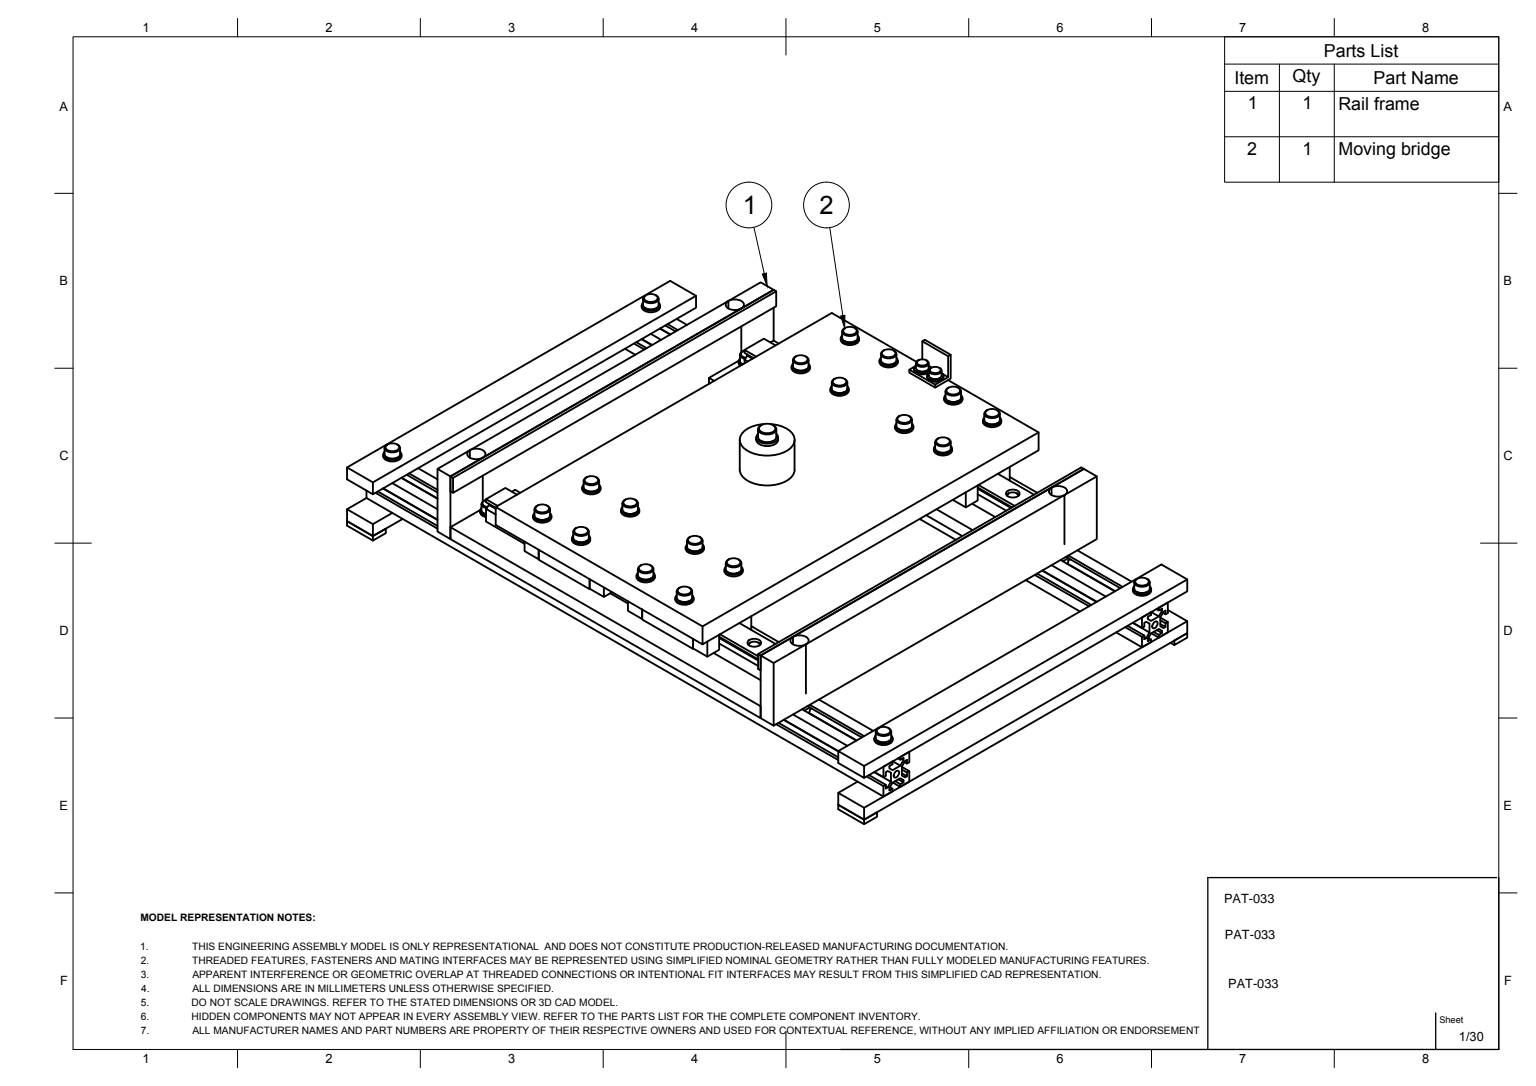
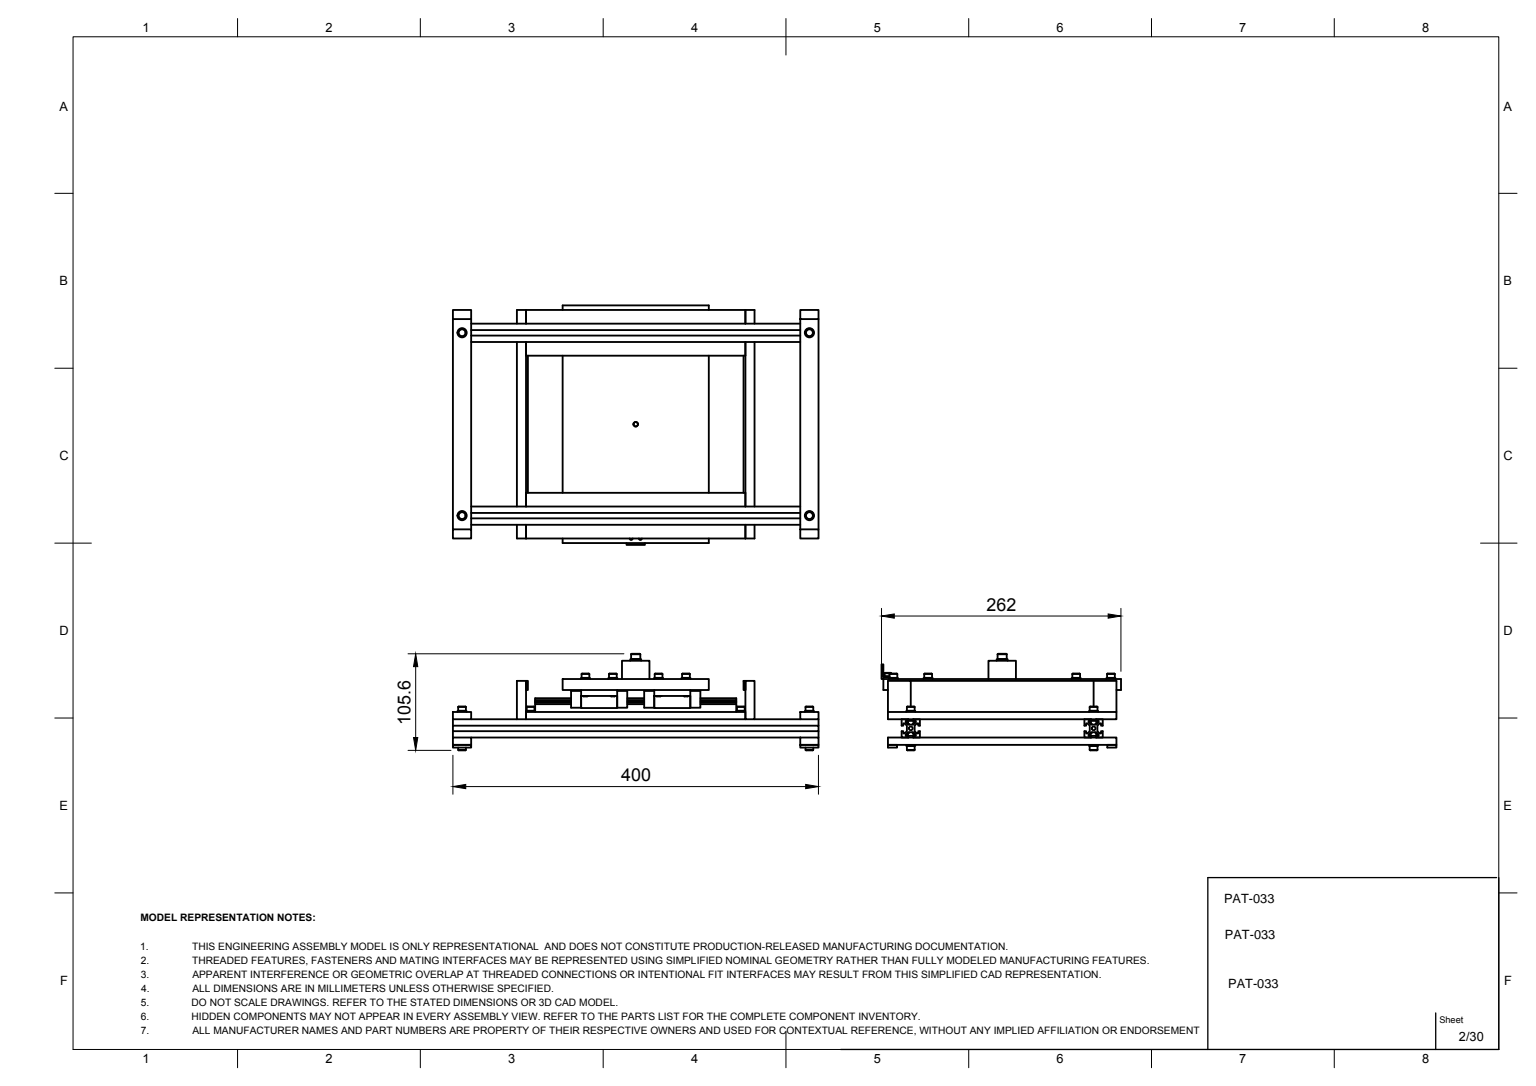
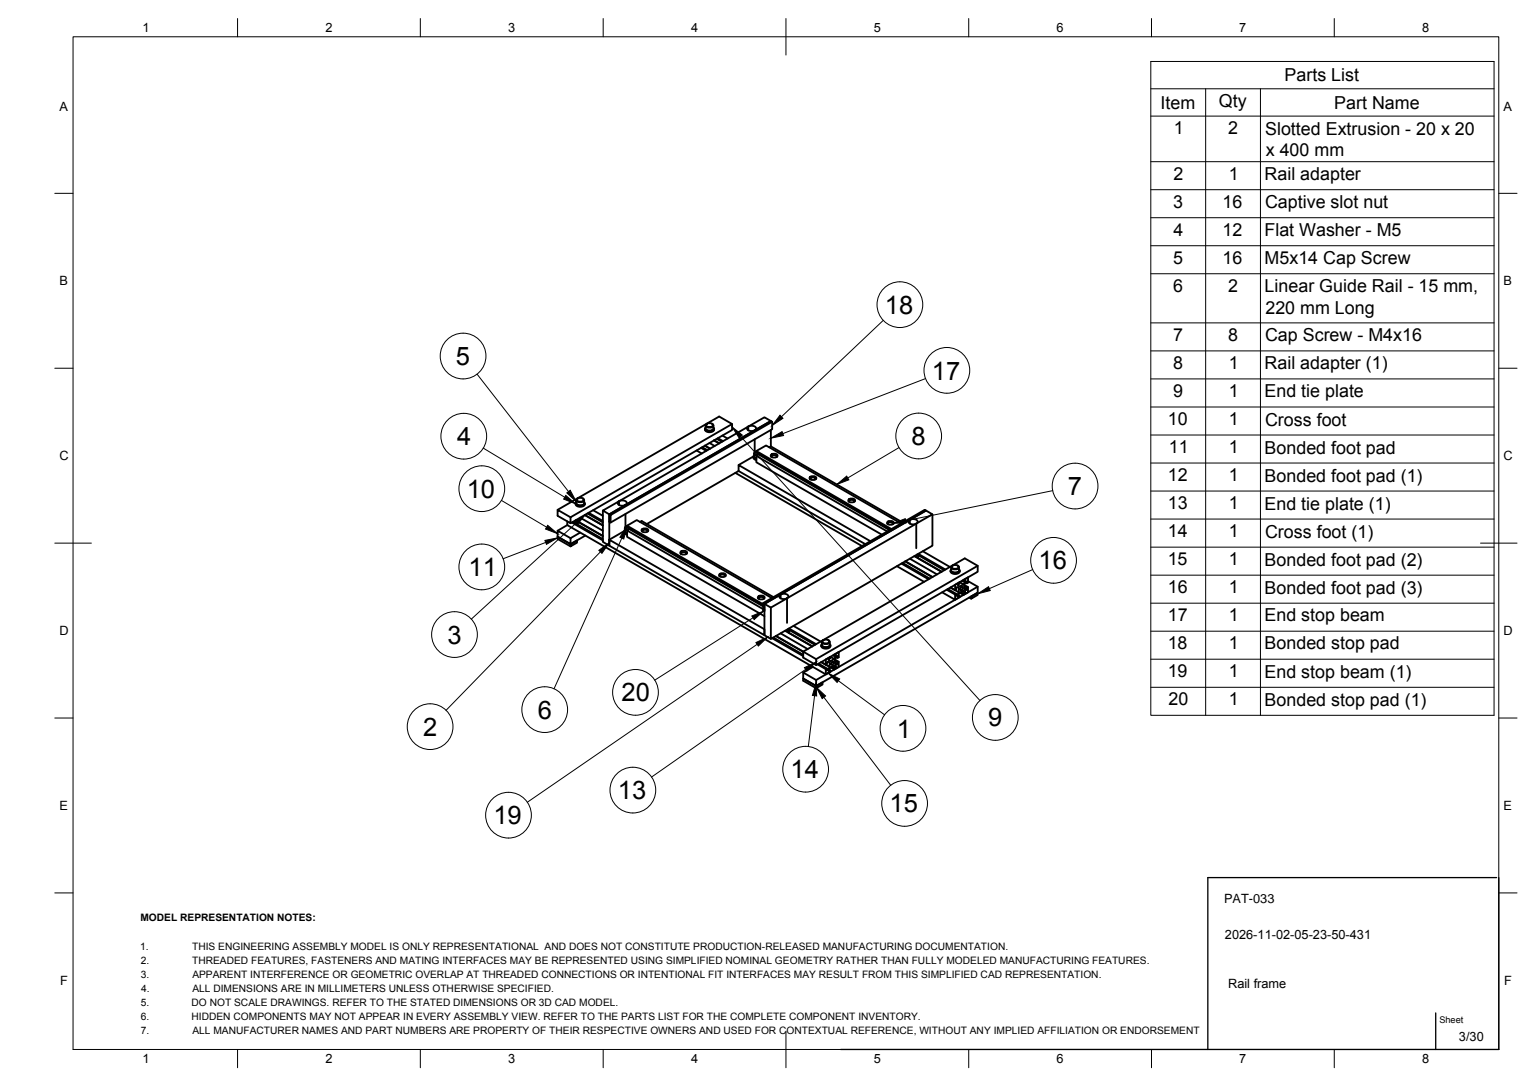
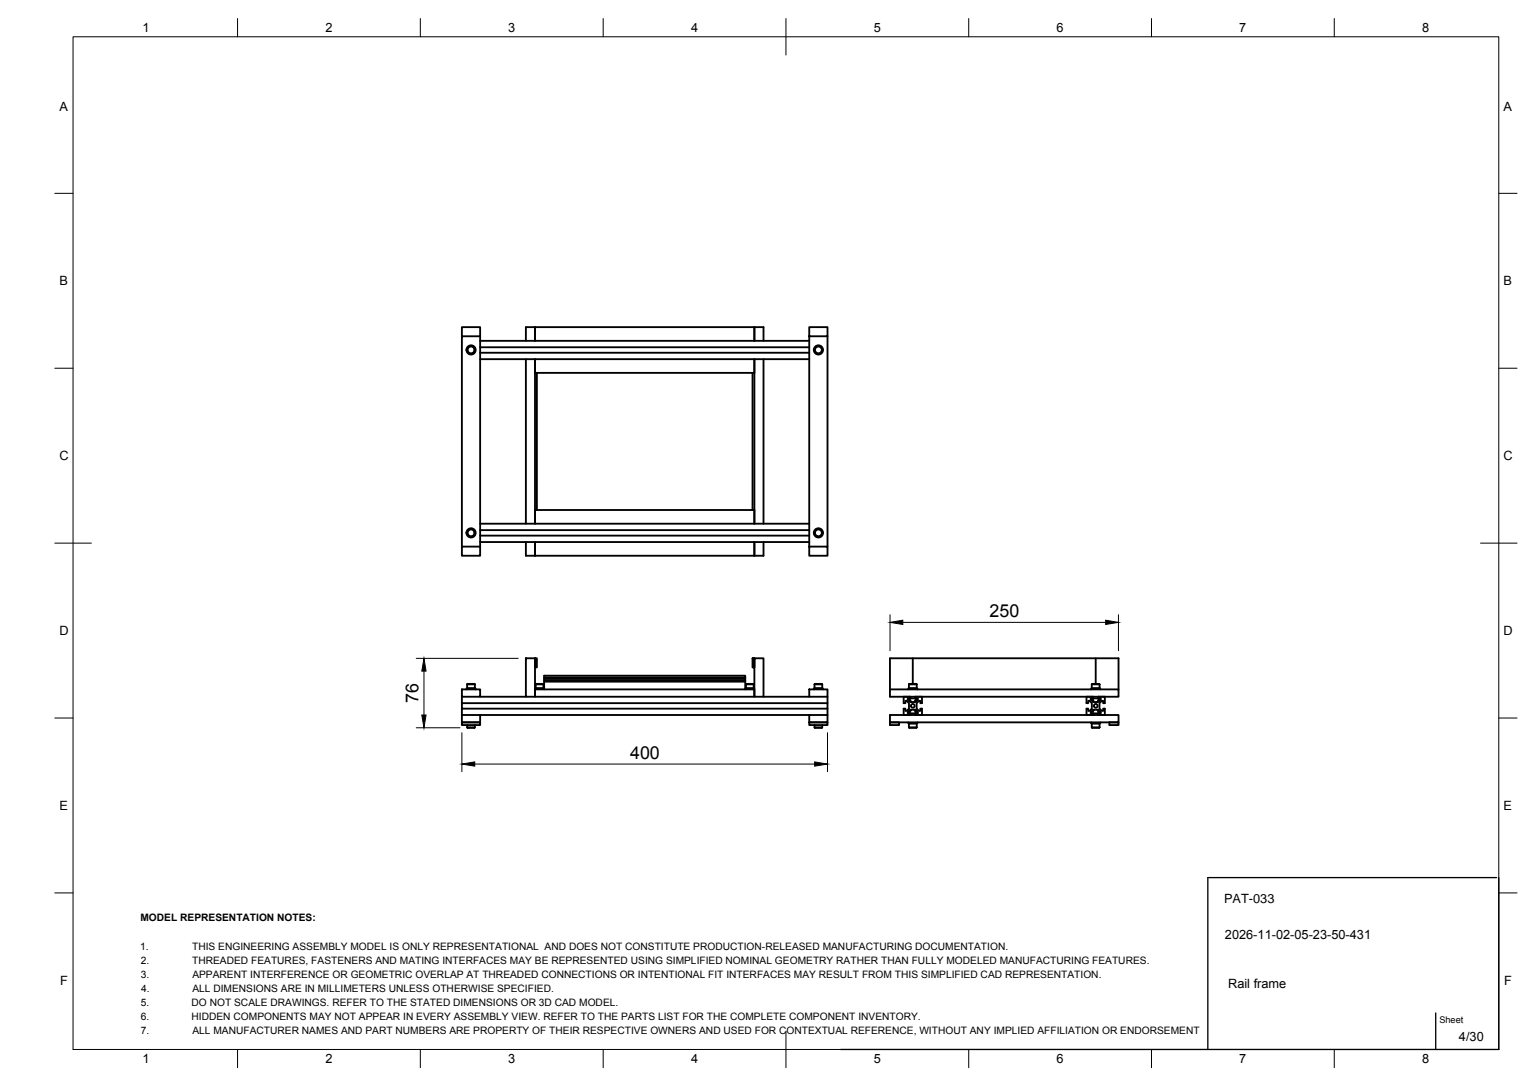
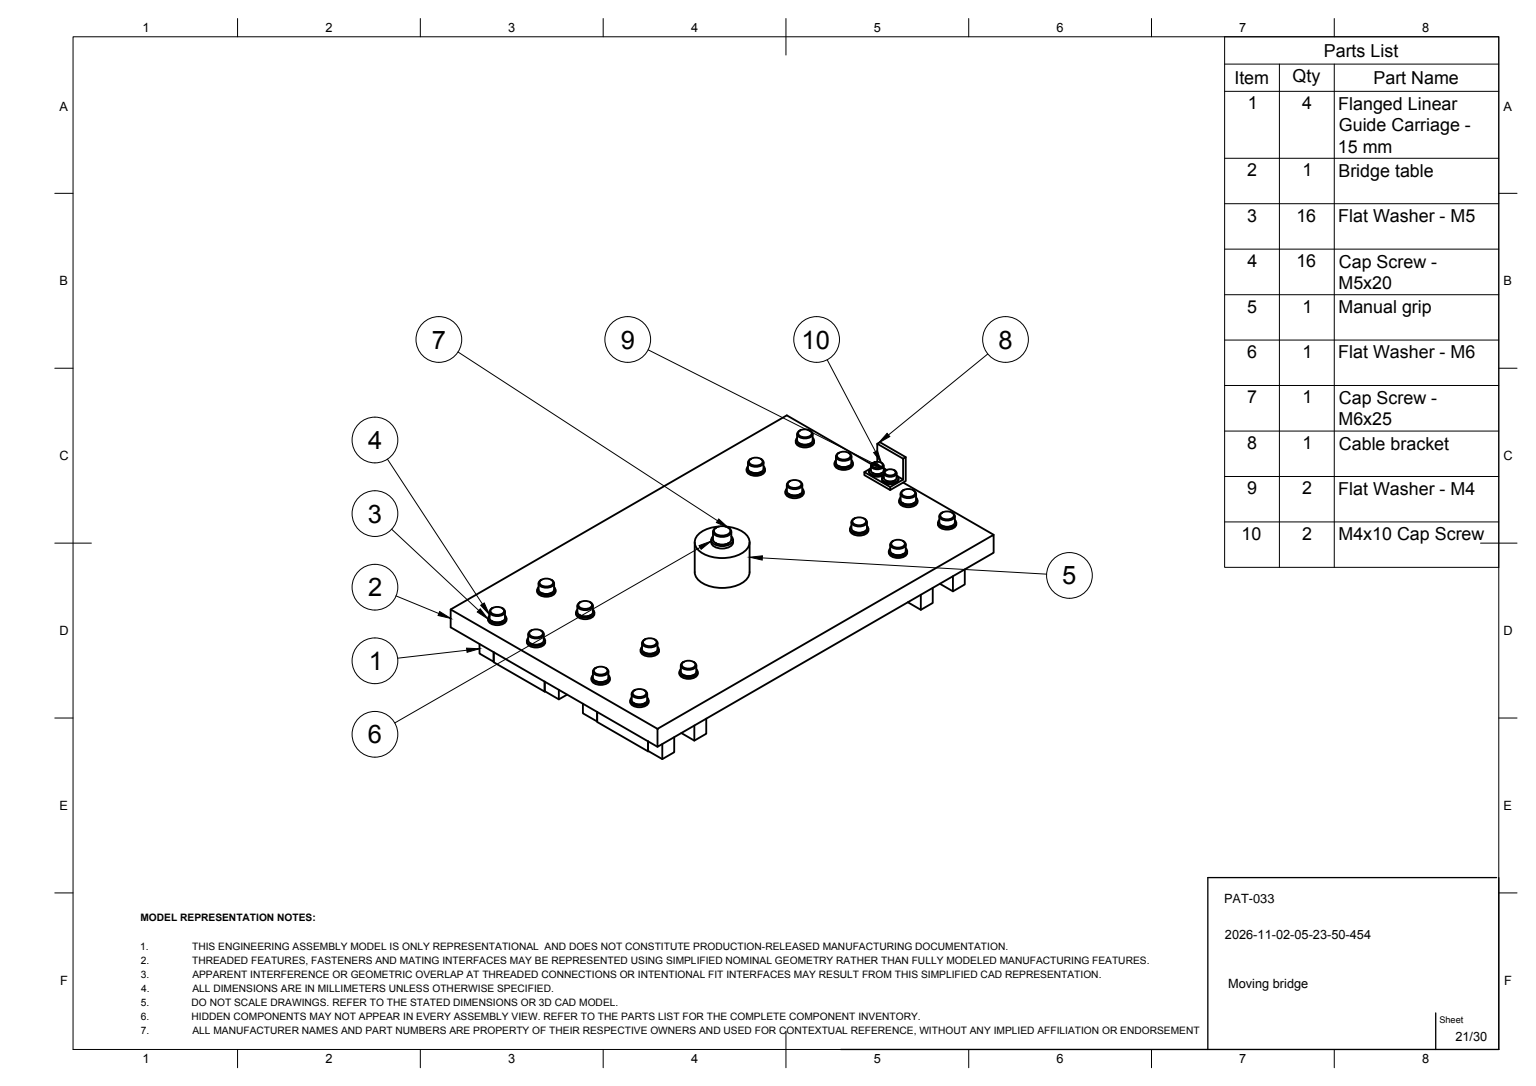
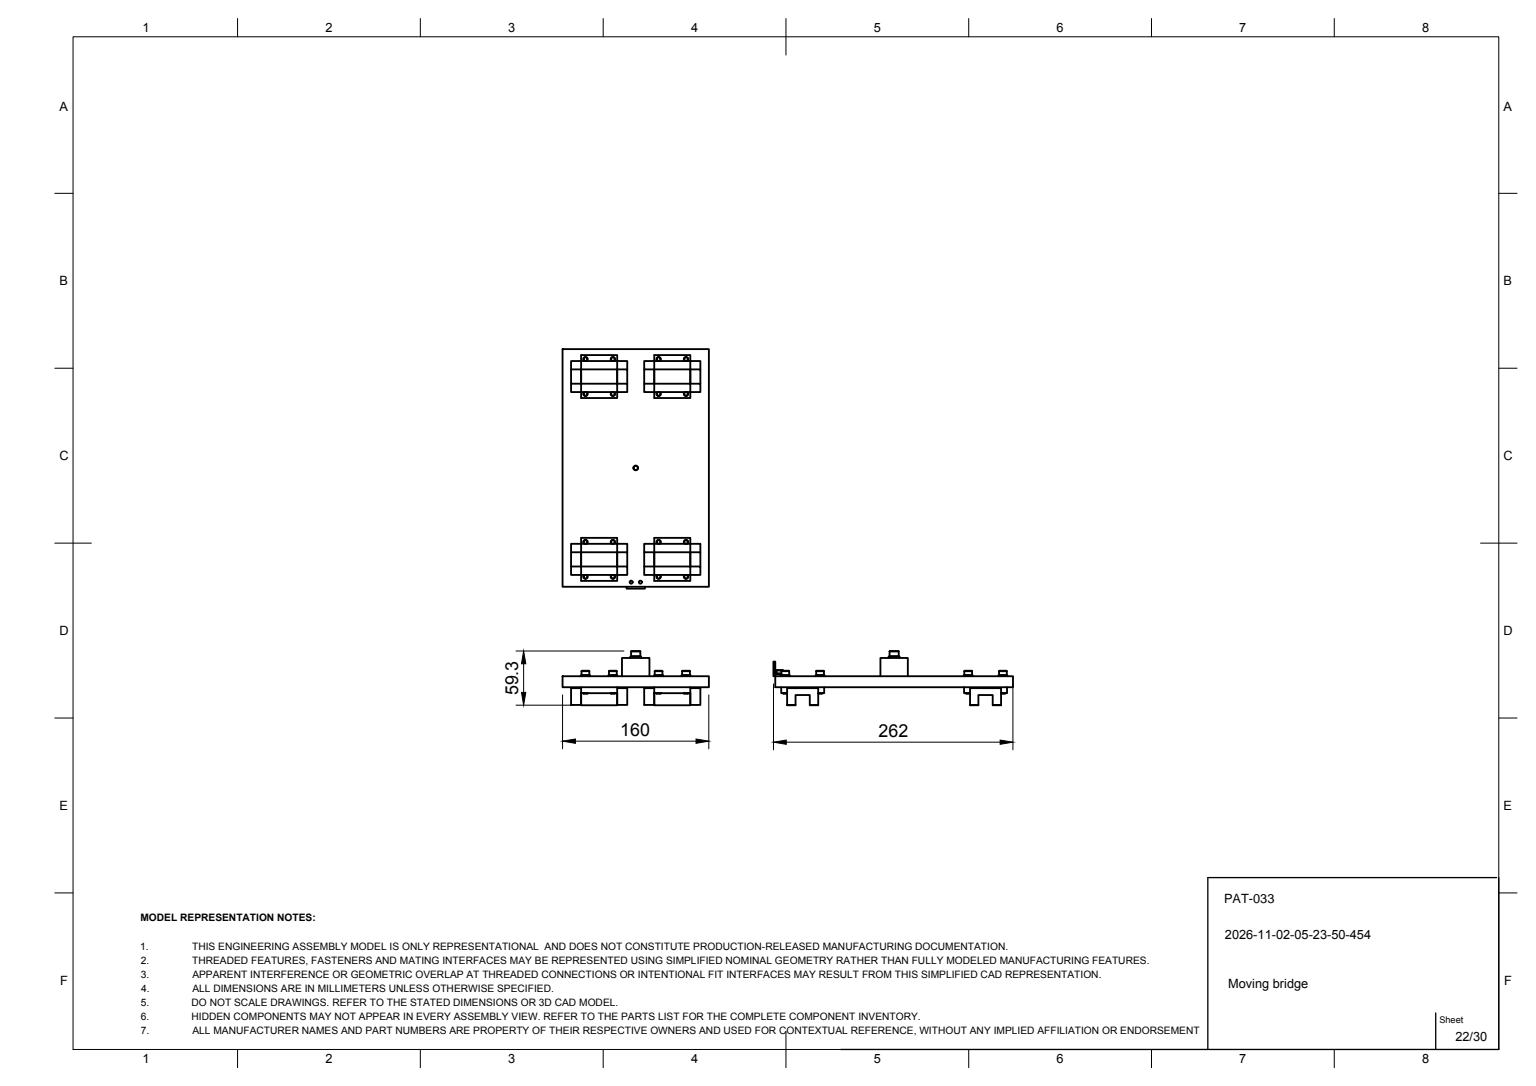
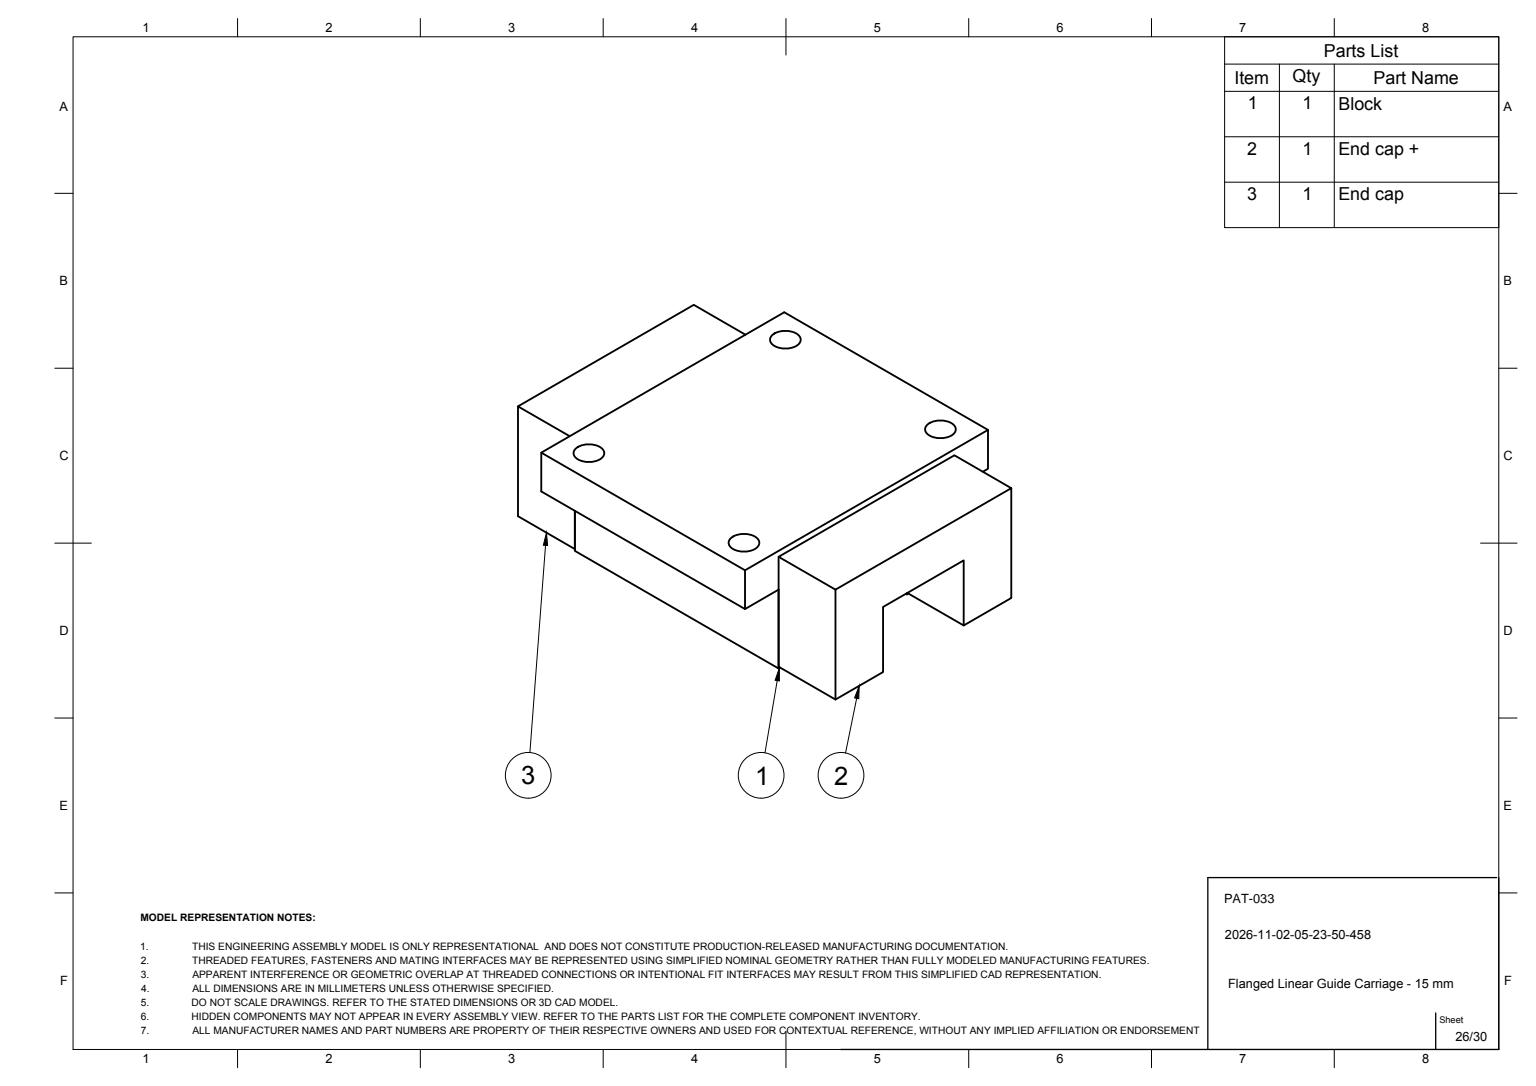
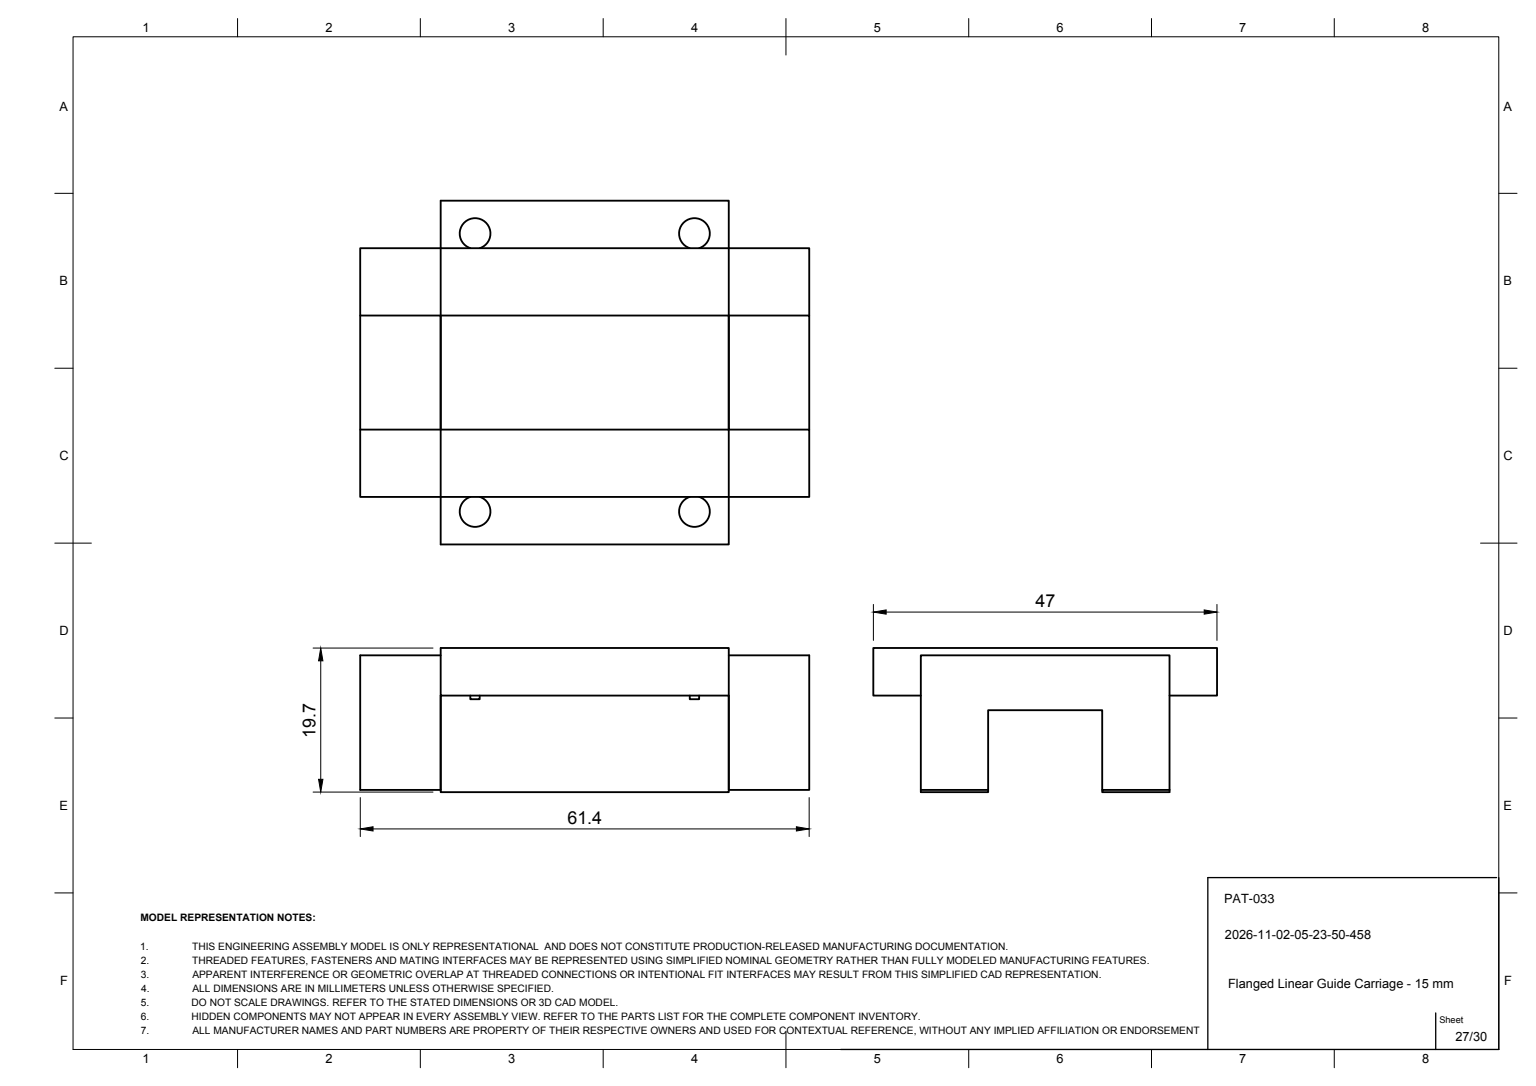
ISO-10303-21;
HEADER;
/* Generated by software containing ST-Developer
 * from STEP Tools, Inc. (www.steptools.com) 
 */

FILE_DESCRIPTION(
/* description */ ('Dual-rail gantry carriage'),
/* implementation_level */ '2;1');

FILE_NAME(
/* name */ 'PAT-033',
/* time_stamp */ '2026-10-27T10:49:15-07:00',
/* author */ (''),
/* organization */ (''),
/* preprocessor_version */ 'ST-DEVELOPER v20.2',
/* originating_system */ 'Autodesk Translation Framework v15.17.0.0',
/* authorisation */ '');

FILE_SCHEMA (('AUTOMOTIVE_DESIGN { 1 0 10303 214 3 1 1 }'));
ENDSEC;

DATA;
#10=MECHANICAL_DESIGN_GEOMETRIC_PRESENTATION_REPRESENTATION('',(#585,#586,
#587,#588,#589,#590,#591,#592,#593,#594,#595,#596,#597,#598,#599,#600,#601,
#602,#603,#604,#605,#606,#607,#608,#609,#610,#611,#612,#613,#614,#615),
#12804);
#11=ITEM_DEFINED_TRANSFORMATION($,$,#8199,#8260);
#12=ITEM_DEFINED_TRANSFORMATION($,$,#8238,#8261);
#13=ITEM_DEFINED_TRANSFORMATION($,$,#8249,#8262);
#14=ITEM_DEFINED_TRANSFORMATION($,$,#7743,#8274);
#15=ITEM_DEFINED_TRANSFORMATION($,$,#7768,#8275);
#16=ITEM_DEFINED_TRANSFORMATION($,$,#7793,#8276);
#17=ITEM_DEFINED_TRANSFORMATION($,$,#7806,#8277);
#18=ITEM_DEFINED_TRANSFORMATION($,$,#7819,#8278);
#19=ITEM_DEFINED_TRANSFORMATION($,$,#7826,#8279);
#20=ITEM_DEFINED_TRANSFORMATION($,$,#7833,#8280);
#21=ITEM_DEFINED_TRANSFORMATION($,$,#7846,#8281);
#22=ITEM_DEFINED_TRANSFORMATION($,$,#7859,#8282);
#23=ITEM_DEFINED_TRANSFORMATION($,$,#7866,#8283);
#24=ITEM_DEFINED_TRANSFORMATION($,$,#7873,#8284);
#25=ITEM_DEFINED_TRANSFORMATION($,$,#7902,#8285);
#26=ITEM_DEFINED_TRANSFORMATION($,$,#7909,#8286);
#27=ITEM_DEFINED_TRANSFORMATION($,$,#7938,#8287);
#28=ITEM_DEFINED_TRANSFORMATION($,$,#7945,#8288);
#29=ITEM_DEFINED_TRANSFORMATION($,$,#8064,#8289);
#30=ITEM_DEFINED_TRANSFORMATION($,$,#8263,#8290);
#31=ITEM_DEFINED_TRANSFORMATION($,$,#8085,#8291);
#32=ITEM_DEFINED_TRANSFORMATION($,$,#8064,#8292);
#33=ITEM_DEFINED_TRANSFORMATION($,$,#8263,#8293);
#34=ITEM_DEFINED_TRANSFORMATION($,$,#8085,#8294);
#35=ITEM_DEFINED_TRANSFORMATION($,$,#7995,#8295);
#36=ITEM_DEFINED_TRANSFORMATION($,$,#8038,#8296);
#37=ITEM_DEFINED_TRANSFORMATION($,$,#8038,#8297);
#38=ITEM_DEFINED_TRANSFORMATION($,$,#8038,#8298);
#39=ITEM_DEFINED_TRANSFORMATION($,$,#8038,#8299);
#40=ITEM_DEFINED_TRANSFORMATION($,$,#7945,#8300);
#41=ITEM_DEFINED_TRANSFORMATION($,$,#8064,#8301);
#42=ITEM_DEFINED_TRANSFORMATION($,$,#8263,#8302);
#43=ITEM_DEFINED_TRANSFORMATION($,$,#8085,#8303);
#44=ITEM_DEFINED_TRANSFORMATION($,$,#8064,#8304);
#45=ITEM_DEFINED_TRANSFORMATION($,$,#8263,#8305);
#46=ITEM_DEFINED_TRANSFORMATION($,$,#8085,#8306);
#47=ITEM_DEFINED_TRANSFORMATION($,$,#7995,#8307);
#48=ITEM_DEFINED_TRANSFORMATION($,$,#8038,#8308);
#49=ITEM_DEFINED_TRANSFORMATION($,$,#8038,#8309);
#50=ITEM_DEFINED_TRANSFORMATION($,$,#8038,#8310);
#51=ITEM_DEFINED_TRANSFORMATION($,$,#8038,#8311);
#52=ITEM_DEFINED_TRANSFORMATION($,$,#8064,#8312);
#53=ITEM_DEFINED_TRANSFORMATION($,$,#8263,#8313);
#54=ITEM_DEFINED_TRANSFORMATION($,$,#8085,#8314);
#55=ITEM_DEFINED_TRANSFORMATION($,$,#8064,#8315);
#56=ITEM_DEFINED_TRANSFORMATION($,$,#8263,#8316);
#57=ITEM_DEFINED_TRANSFORMATION($,$,#8085,#8317);
#58=ITEM_DEFINED_TRANSFORMATION($,$,#8064,#8318);
#59=ITEM_DEFINED_TRANSFORMATION($,$,#8263,#8319);
#60=ITEM_DEFINED_TRANSFORMATION($,$,#8085,#8320);
#61=ITEM_DEFINED_TRANSFORMATION($,$,#8064,#8321);
#62=ITEM_DEFINED_TRANSFORMATION($,$,#8263,#8322);
#63=ITEM_DEFINED_TRANSFORMATION($,$,#8085,#8323);
#64=ITEM_DEFINED_TRANSFORMATION($,$,#8064,#8324);
#65=ITEM_DEFINED_TRANSFORMATION($,$,#8263,#8325);
#66=ITEM_DEFINED_TRANSFORMATION($,$,#8085,#8326);
#67=ITEM_DEFINED_TRANSFORMATION($,$,#8064,#8327);
#68=ITEM_DEFINED_TRANSFORMATION($,$,#8263,#8328);
#69=ITEM_DEFINED_TRANSFORMATION($,$,#8085,#8329);
#70=ITEM_DEFINED_TRANSFORMATION($,$,#8064,#8330);
#71=ITEM_DEFINED_TRANSFORMATION($,$,#8263,#8331);
#72=ITEM_DEFINED_TRANSFORMATION($,$,#8085,#8332);
#73=ITEM_DEFINED_TRANSFORMATION($,$,#8064,#8333);
#74=ITEM_DEFINED_TRANSFORMATION($,$,#8263,#8334);
#75=ITEM_DEFINED_TRANSFORMATION($,$,#8085,#8335);
#76=ITEM_DEFINED_TRANSFORMATION($,$,#8064,#8336);
#77=ITEM_DEFINED_TRANSFORMATION($,$,#8085,#8337);
#78=ITEM_DEFINED_TRANSFORMATION($,$,#8064,#8338);
#79=ITEM_DEFINED_TRANSFORMATION($,$,#8085,#8339);
#80=ITEM_DEFINED_TRANSFORMATION($,$,#8064,#8340);
#81=ITEM_DEFINED_TRANSFORMATION($,$,#8085,#8341);
#82=ITEM_DEFINED_TRANSFORMATION($,$,#8064,#8342);
#83=ITEM_DEFINED_TRANSFORMATION($,$,#8085,#8343);
#84=ITEM_DEFINED_TRANSFORMATION($,$,#8110,#8440);
#85=ITEM_DEFINED_TRANSFORMATION($,$,#8174,#8441);
#86=ITEM_DEFINED_TRANSFORMATION($,$,#8183,#8442);
#87=ITEM_DEFINED_TRANSFORMATION($,$,#8198,#8443);
#88=ITEM_DEFINED_TRANSFORMATION($,$,#8198,#8444);
#89=ITEM_DEFINED_TRANSFORMATION($,$,#8198,#8445);
#90=ITEM_DEFINED_TRANSFORMATION($,$,#8198,#8446);
#91=ITEM_DEFINED_TRANSFORMATION($,$,#8263,#8447);
#92=ITEM_DEFINED_TRANSFORMATION($,$,#8344,#8448);
#93=ITEM_DEFINED_TRANSFORMATION($,$,#8263,#8449);
#94=ITEM_DEFINED_TRANSFORMATION($,$,#8344,#8450);
#95=ITEM_DEFINED_TRANSFORMATION($,$,#8263,#8451);
#96=ITEM_DEFINED_TRANSFORMATION($,$,#8344,#8452);
#97=ITEM_DEFINED_TRANSFORMATION($,$,#8263,#8453);
#98=ITEM_DEFINED_TRANSFORMATION($,$,#8344,#8454);
#99=ITEM_DEFINED_TRANSFORMATION($,$,#8263,#8455);
#100=ITEM_DEFINED_TRANSFORMATION($,$,#8344,#8456);
#101=ITEM_DEFINED_TRANSFORMATION($,$,#8263,#8457);
#102=ITEM_DEFINED_TRANSFORMATION($,$,#8344,#8458);
#103=ITEM_DEFINED_TRANSFORMATION($,$,#8263,#8459);
#104=ITEM_DEFINED_TRANSFORMATION($,$,#8344,#8460);
#105=ITEM_DEFINED_TRANSFORMATION($,$,#8263,#8461);
#106=ITEM_DEFINED_TRANSFORMATION($,$,#8344,#8462);
#107=ITEM_DEFINED_TRANSFORMATION($,$,#8263,#8463);
#108=ITEM_DEFINED_TRANSFORMATION($,$,#8344,#8464);
#109=ITEM_DEFINED_TRANSFORMATION($,$,#8263,#8465);
#110=ITEM_DEFINED_TRANSFORMATION($,$,#8344,#8466);
#111=ITEM_DEFINED_TRANSFORMATION($,$,#8263,#8467);
#112=ITEM_DEFINED_TRANSFORMATION($,$,#8344,#8468);
#113=ITEM_DEFINED_TRANSFORMATION($,$,#8263,#8469);
#114=ITEM_DEFINED_TRANSFORMATION($,$,#8344,#8470);
#115=ITEM_DEFINED_TRANSFORMATION($,$,#8263,#8471);
#116=ITEM_DEFINED_TRANSFORMATION($,$,#8344,#8472);
#117=ITEM_DEFINED_TRANSFORMATION($,$,#8263,#8473);
#118=ITEM_DEFINED_TRANSFORMATION($,$,#8344,#8474);
#119=ITEM_DEFINED_TRANSFORMATION($,$,#8263,#8475);
#120=ITEM_DEFINED_TRANSFORMATION($,$,#8344,#8476);
#121=ITEM_DEFINED_TRANSFORMATION($,$,#8263,#8477);
#122=ITEM_DEFINED_TRANSFORMATION($,$,#8344,#8478);
#123=ITEM_DEFINED_TRANSFORMATION($,$,#8370,#8479);
#124=ITEM_DEFINED_TRANSFORMATION($,$,#8379,#8480);
#125=ITEM_DEFINED_TRANSFORMATION($,$,#8405,#8481);
#126=ITEM_DEFINED_TRANSFORMATION($,$,#8416,#8482);
#127=ITEM_DEFINED_TRANSFORMATION($,$,#8405,#8483);
#128=ITEM_DEFINED_TRANSFORMATION($,$,#8416,#8484);
#129=ITEM_DEFINED_TRANSFORMATION($,$,#7742,#8485);
#130=ITEM_DEFINED_TRANSFORMATION($,$,#8109,#8486);
#131=(
REPRESENTATION_RELATIONSHIP($,$,#13025,#13024)
REPRESENTATION_RELATIONSHIP_WITH_TRANSFORMATION(#11)
SHAPE_REPRESENTATION_RELATIONSHIP()
);
#132=(
REPRESENTATION_RELATIONSHIP($,$,#13026,#13024)
REPRESENTATION_RELATIONSHIP_WITH_TRANSFORMATION(#12)
SHAPE_REPRESENTATION_RELATIONSHIP()
);
#133=(
REPRESENTATION_RELATIONSHIP($,$,#13027,#13024)
REPRESENTATION_RELATIONSHIP_WITH_TRANSFORMATION(#13)
SHAPE_REPRESENTATION_RELATIONSHIP()
);
#134=(
REPRESENTATION_RELATIONSHIP($,$,#13001,#13000)
REPRESENTATION_RELATIONSHIP_WITH_TRANSFORMATION(#14)
SHAPE_REPRESENTATION_RELATIONSHIP()
);
#135=(
REPRESENTATION_RELATIONSHIP($,$,#13002,#13000)
REPRESENTATION_RELATIONSHIP_WITH_TRANSFORMATION(#15)
SHAPE_REPRESENTATION_RELATIONSHIP()
);
#136=(
REPRESENTATION_RELATIONSHIP($,$,#13003,#13000)
REPRESENTATION_RELATIONSHIP_WITH_TRANSFORMATION(#16)
SHAPE_REPRESENTATION_RELATIONSHIP()
);
#137=(
REPRESENTATION_RELATIONSHIP($,$,#13004,#13000)
REPRESENTATION_RELATIONSHIP_WITH_TRANSFORMATION(#17)
SHAPE_REPRESENTATION_RELATIONSHIP()
);
#138=(
REPRESENTATION_RELATIONSHIP($,$,#13005,#13000)
REPRESENTATION_RELATIONSHIP_WITH_TRANSFORMATION(#18)
SHAPE_REPRESENTATION_RELATIONSHIP()
);
#139=(
REPRESENTATION_RELATIONSHIP($,$,#13006,#13000)
REPRESENTATION_RELATIONSHIP_WITH_TRANSFORMATION(#19)
SHAPE_REPRESENTATION_RELATIONSHIP()
);
#140=(
REPRESENTATION_RELATIONSHIP($,$,#13007,#13000)
REPRESENTATION_RELATIONSHIP_WITH_TRANSFORMATION(#20)
SHAPE_REPRESENTATION_RELATIONSHIP()
);
#141=(
REPRESENTATION_RELATIONSHIP($,$,#13008,#13000)
REPRESENTATION_RELATIONSHIP_WITH_TRANSFORMATION(#21)
SHAPE_REPRESENTATION_RELATIONSHIP()
);
#142=(
REPRESENTATION_RELATIONSHIP($,$,#13009,#13000)
REPRESENTATION_RELATIONSHIP_WITH_TRANSFORMATION(#22)
SHAPE_REPRESENTATION_RELATIONSHIP()
);
#143=(
REPRESENTATION_RELATIONSHIP($,$,#13010,#13000)
REPRESENTATION_RELATIONSHIP_WITH_TRANSFORMATION(#23)
SHAPE_REPRESENTATION_RELATIONSHIP()
);
#144=(
REPRESENTATION_RELATIONSHIP($,$,#13011,#13000)
REPRESENTATION_RELATIONSHIP_WITH_TRANSFORMATION(#24)
SHAPE_REPRESENTATION_RELATIONSHIP()
);
#145=(
REPRESENTATION_RELATIONSHIP($,$,#13012,#13000)
REPRESENTATION_RELATIONSHIP_WITH_TRANSFORMATION(#25)
SHAPE_REPRESENTATION_RELATIONSHIP()
);
#146=(
REPRESENTATION_RELATIONSHIP($,$,#13013,#13000)
REPRESENTATION_RELATIONSHIP_WITH_TRANSFORMATION(#26)
SHAPE_REPRESENTATION_RELATIONSHIP()
);
#147=(
REPRESENTATION_RELATIONSHIP($,$,#13014,#13000)
REPRESENTATION_RELATIONSHIP_WITH_TRANSFORMATION(#27)
SHAPE_REPRESENTATION_RELATIONSHIP()
);
#148=(
REPRESENTATION_RELATIONSHIP($,$,#13015,#13000)
REPRESENTATION_RELATIONSHIP_WITH_TRANSFORMATION(#28)
SHAPE_REPRESENTATION_RELATIONSHIP()
);
#149=(
REPRESENTATION_RELATIONSHIP($,$,#13018,#13000)
REPRESENTATION_RELATIONSHIP_WITH_TRANSFORMATION(#29)
SHAPE_REPRESENTATION_RELATIONSHIP()
);
#150=(
REPRESENTATION_RELATIONSHIP($,$,#13028,#13000)
REPRESENTATION_RELATIONSHIP_WITH_TRANSFORMATION(#30)
SHAPE_REPRESENTATION_RELATIONSHIP()
);
#151=(
REPRESENTATION_RELATIONSHIP($,$,#13019,#13000)
REPRESENTATION_RELATIONSHIP_WITH_TRANSFORMATION(#31)
SHAPE_REPRESENTATION_RELATIONSHIP()
);
#152=(
REPRESENTATION_RELATIONSHIP($,$,#13018,#13000)
REPRESENTATION_RELATIONSHIP_WITH_TRANSFORMATION(#32)
SHAPE_REPRESENTATION_RELATIONSHIP()
);
#153=(
REPRESENTATION_RELATIONSHIP($,$,#13028,#13000)
REPRESENTATION_RELATIONSHIP_WITH_TRANSFORMATION(#33)
SHAPE_REPRESENTATION_RELATIONSHIP()
);
#154=(
REPRESENTATION_RELATIONSHIP($,$,#13019,#13000)
REPRESENTATION_RELATIONSHIP_WITH_TRANSFORMATION(#34)
SHAPE_REPRESENTATION_RELATIONSHIP()
);
#155=(
REPRESENTATION_RELATIONSHIP($,$,#13016,#13000)
REPRESENTATION_RELATIONSHIP_WITH_TRANSFORMATION(#35)
SHAPE_REPRESENTATION_RELATIONSHIP()
);
#156=(
REPRESENTATION_RELATIONSHIP($,$,#13017,#13000)
REPRESENTATION_RELATIONSHIP_WITH_TRANSFORMATION(#36)
SHAPE_REPRESENTATION_RELATIONSHIP()
);
#157=(
REPRESENTATION_RELATIONSHIP($,$,#13017,#13000)
REPRESENTATION_RELATIONSHIP_WITH_TRANSFORMATION(#37)
SHAPE_REPRESENTATION_RELATIONSHIP()
);
#158=(
REPRESENTATION_RELATIONSHIP($,$,#13017,#13000)
REPRESENTATION_RELATIONSHIP_WITH_TRANSFORMATION(#38)
SHAPE_REPRESENTATION_RELATIONSHIP()
);
#159=(
REPRESENTATION_RELATIONSHIP($,$,#13017,#13000)
REPRESENTATION_RELATIONSHIP_WITH_TRANSFORMATION(#39)
SHAPE_REPRESENTATION_RELATIONSHIP()
);
#160=(
REPRESENTATION_RELATIONSHIP($,$,#13015,#13000)
REPRESENTATION_RELATIONSHIP_WITH_TRANSFORMATION(#40)
SHAPE_REPRESENTATION_RELATIONSHIP()
);
#161=(
REPRESENTATION_RELATIONSHIP($,$,#13018,#13000)
REPRESENTATION_RELATIONSHIP_WITH_TRANSFORMATION(#41)
SHAPE_REPRESENTATION_RELATIONSHIP()
);
#162=(
REPRESENTATION_RELATIONSHIP($,$,#13028,#13000)
REPRESENTATION_RELATIONSHIP_WITH_TRANSFORMATION(#42)
SHAPE_REPRESENTATION_RELATIONSHIP()
);
#163=(
REPRESENTATION_RELATIONSHIP($,$,#13019,#13000)
REPRESENTATION_RELATIONSHIP_WITH_TRANSFORMATION(#43)
SHAPE_REPRESENTATION_RELATIONSHIP()
);
#164=(
REPRESENTATION_RELATIONSHIP($,$,#13018,#13000)
REPRESENTATION_RELATIONSHIP_WITH_TRANSFORMATION(#44)
SHAPE_REPRESENTATION_RELATIONSHIP()
);
#165=(
REPRESENTATION_RELATIONSHIP($,$,#13028,#13000)
REPRESENTATION_RELATIONSHIP_WITH_TRANSFORMATION(#45)
SHAPE_REPRESENTATION_RELATIONSHIP()
);
#166=(
REPRESENTATION_RELATIONSHIP($,$,#13019,#13000)
REPRESENTATION_RELATIONSHIP_WITH_TRANSFORMATION(#46)
SHAPE_REPRESENTATION_RELATIONSHIP()
);
#167=(
REPRESENTATION_RELATIONSHIP($,$,#13016,#13000)
REPRESENTATION_RELATIONSHIP_WITH_TRANSFORMATION(#47)
SHAPE_REPRESENTATION_RELATIONSHIP()
);
#168=(
REPRESENTATION_RELATIONSHIP($,$,#13017,#13000)
REPRESENTATION_RELATIONSHIP_WITH_TRANSFORMATION(#48)
SHAPE_REPRESENTATION_RELATIONSHIP()
);
#169=(
REPRESENTATION_RELATIONSHIP($,$,#13017,#13000)
REPRESENTATION_RELATIONSHIP_WITH_TRANSFORMATION(#49)
SHAPE_REPRESENTATION_RELATIONSHIP()
);
#170=(
REPRESENTATION_RELATIONSHIP($,$,#13017,#13000)
REPRESENTATION_RELATIONSHIP_WITH_TRANSFORMATION(#50)
SHAPE_REPRESENTATION_RELATIONSHIP()
);
#171=(
REPRESENTATION_RELATIONSHIP($,$,#13017,#13000)
REPRESENTATION_RELATIONSHIP_WITH_TRANSFORMATION(#51)
SHAPE_REPRESENTATION_RELATIONSHIP()
);
#172=(
REPRESENTATION_RELATIONSHIP($,$,#13018,#13000)
REPRESENTATION_RELATIONSHIP_WITH_TRANSFORMATION(#52)
SHAPE_REPRESENTATION_RELATIONSHIP()
);
#173=(
REPRESENTATION_RELATIONSHIP($,$,#13028,#13000)
REPRESENTATION_RELATIONSHIP_WITH_TRANSFORMATION(#53)
SHAPE_REPRESENTATION_RELATIONSHIP()
);
#174=(
REPRESENTATION_RELATIONSHIP($,$,#13019,#13000)
REPRESENTATION_RELATIONSHIP_WITH_TRANSFORMATION(#54)
SHAPE_REPRESENTATION_RELATIONSHIP()
);
#175=(
REPRESENTATION_RELATIONSHIP($,$,#13018,#13000)
REPRESENTATION_RELATIONSHIP_WITH_TRANSFORMATION(#55)
SHAPE_REPRESENTATION_RELATIONSHIP()
);
#176=(
REPRESENTATION_RELATIONSHIP($,$,#13028,#13000)
REPRESENTATION_RELATIONSHIP_WITH_TRANSFORMATION(#56)
SHAPE_REPRESENTATION_RELATIONSHIP()
);
#177=(
REPRESENTATION_RELATIONSHIP($,$,#13019,#13000)
REPRESENTATION_RELATIONSHIP_WITH_TRANSFORMATION(#57)
SHAPE_REPRESENTATION_RELATIONSHIP()
);
#178=(
REPRESENTATION_RELATIONSHIP($,$,#13018,#13000)
REPRESENTATION_RELATIONSHIP_WITH_TRANSFORMATION(#58)
SHAPE_REPRESENTATION_RELATIONSHIP()
);
#179=(
REPRESENTATION_RELATIONSHIP($,$,#13028,#13000)
REPRESENTATION_RELATIONSHIP_WITH_TRANSFORMATION(#59)
SHAPE_REPRESENTATION_RELATIONSHIP()
);
#180=(
REPRESENTATION_RELATIONSHIP($,$,#13019,#13000)
REPRESENTATION_RELATIONSHIP_WITH_TRANSFORMATION(#60)
SHAPE_REPRESENTATION_RELATIONSHIP()
);
#181=(
REPRESENTATION_RELATIONSHIP($,$,#13018,#13000)
REPRESENTATION_RELATIONSHIP_WITH_TRANSFORMATION(#61)
SHAPE_REPRESENTATION_RELATIONSHIP()
);
#182=(
REPRESENTATION_RELATIONSHIP($,$,#13028,#13000)
REPRESENTATION_RELATIONSHIP_WITH_TRANSFORMATION(#62)
SHAPE_REPRESENTATION_RELATIONSHIP()
);
#183=(
REPRESENTATION_RELATIONSHIP($,$,#13019,#13000)
REPRESENTATION_RELATIONSHIP_WITH_TRANSFORMATION(#63)
SHAPE_REPRESENTATION_RELATIONSHIP()
);
#184=(
REPRESENTATION_RELATIONSHIP($,$,#13018,#13000)
REPRESENTATION_RELATIONSHIP_WITH_TRANSFORMATION(#64)
SHAPE_REPRESENTATION_RELATIONSHIP()
);
#185=(
REPRESENTATION_RELATIONSHIP($,$,#13028,#13000)
REPRESENTATION_RELATIONSHIP_WITH_TRANSFORMATION(#65)
SHAPE_REPRESENTATION_RELATIONSHIP()
);
#186=(
REPRESENTATION_RELATIONSHIP($,$,#13019,#13000)
REPRESENTATION_RELATIONSHIP_WITH_TRANSFORMATION(#66)
SHAPE_REPRESENTATION_RELATIONSHIP()
);
#187=(
REPRESENTATION_RELATIONSHIP($,$,#13018,#13000)
REPRESENTATION_RELATIONSHIP_WITH_TRANSFORMATION(#67)
SHAPE_REPRESENTATION_RELATIONSHIP()
);
#188=(
REPRESENTATION_RELATIONSHIP($,$,#13028,#13000)
REPRESENTATION_RELATIONSHIP_WITH_TRANSFORMATION(#68)
SHAPE_REPRESENTATION_RELATIONSHIP()
);
#189=(
REPRESENTATION_RELATIONSHIP($,$,#13019,#13000)
REPRESENTATION_RELATIONSHIP_WITH_TRANSFORMATION(#69)
SHAPE_REPRESENTATION_RELATIONSHIP()
);
#190=(
REPRESENTATION_RELATIONSHIP($,$,#13018,#13000)
REPRESENTATION_RELATIONSHIP_WITH_TRANSFORMATION(#70)
SHAPE_REPRESENTATION_RELATIONSHIP()
);
#191=(
REPRESENTATION_RELATIONSHIP($,$,#13028,#13000)
REPRESENTATION_RELATIONSHIP_WITH_TRANSFORMATION(#71)
SHAPE_REPRESENTATION_RELATIONSHIP()
);
#192=(
REPRESENTATION_RELATIONSHIP($,$,#13019,#13000)
REPRESENTATION_RELATIONSHIP_WITH_TRANSFORMATION(#72)
SHAPE_REPRESENTATION_RELATIONSHIP()
);
#193=(
REPRESENTATION_RELATIONSHIP($,$,#13018,#13000)
REPRESENTATION_RELATIONSHIP_WITH_TRANSFORMATION(#73)
SHAPE_REPRESENTATION_RELATIONSHIP()
);
#194=(
REPRESENTATION_RELATIONSHIP($,$,#13028,#13000)
REPRESENTATION_RELATIONSHIP_WITH_TRANSFORMATION(#74)
SHAPE_REPRESENTATION_RELATIONSHIP()
);
#195=(
REPRESENTATION_RELATIONSHIP($,$,#13019,#13000)
REPRESENTATION_RELATIONSHIP_WITH_TRANSFORMATION(#75)
SHAPE_REPRESENTATION_RELATIONSHIP()
);
#196=(
REPRESENTATION_RELATIONSHIP($,$,#13018,#13000)
REPRESENTATION_RELATIONSHIP_WITH_TRANSFORMATION(#76)
SHAPE_REPRESENTATION_RELATIONSHIP()
);
#197=(
REPRESENTATION_RELATIONSHIP($,$,#13019,#13000)
REPRESENTATION_RELATIONSHIP_WITH_TRANSFORMATION(#77)
SHAPE_REPRESENTATION_RELATIONSHIP()
);
#198=(
REPRESENTATION_RELATIONSHIP($,$,#13018,#13000)
REPRESENTATION_RELATIONSHIP_WITH_TRANSFORMATION(#78)
SHAPE_REPRESENTATION_RELATIONSHIP()
);
#199=(
REPRESENTATION_RELATIONSHIP($,$,#13019,#13000)
REPRESENTATION_RELATIONSHIP_WITH_TRANSFORMATION(#79)
SHAPE_REPRESENTATION_RELATIONSHIP()
);
#200=(
REPRESENTATION_RELATIONSHIP($,$,#13018,#13000)
REPRESENTATION_RELATIONSHIP_WITH_TRANSFORMATION(#80)
SHAPE_REPRESENTATION_RELATIONSHIP()
);
#201=(
REPRESENTATION_RELATIONSHIP($,$,#13019,#13000)
REPRESENTATION_RELATIONSHIP_WITH_TRANSFORMATION(#81)
SHAPE_REPRESENTATION_RELATIONSHIP()
);
#202=(
REPRESENTATION_RELATIONSHIP($,$,#13018,#13000)
REPRESENTATION_RELATIONSHIP_WITH_TRANSFORMATION(#82)
SHAPE_REPRESENTATION_RELATIONSHIP()
);
#203=(
REPRESENTATION_RELATIONSHIP($,$,#13019,#13000)
REPRESENTATION_RELATIONSHIP_WITH_TRANSFORMATION(#83)
SHAPE_REPRESENTATION_RELATIONSHIP()
);
#204=(
REPRESENTATION_RELATIONSHIP($,$,#13021,#13020)
REPRESENTATION_RELATIONSHIP_WITH_TRANSFORMATION(#84)
SHAPE_REPRESENTATION_RELATIONSHIP()
);
#205=(
REPRESENTATION_RELATIONSHIP($,$,#13022,#13020)
REPRESENTATION_RELATIONSHIP_WITH_TRANSFORMATION(#85)
SHAPE_REPRESENTATION_RELATIONSHIP()
);
#206=(
REPRESENTATION_RELATIONSHIP($,$,#13023,#13020)
REPRESENTATION_RELATIONSHIP_WITH_TRANSFORMATION(#86)
SHAPE_REPRESENTATION_RELATIONSHIP()
);
#207=(
REPRESENTATION_RELATIONSHIP($,$,#13024,#13020)
REPRESENTATION_RELATIONSHIP_WITH_TRANSFORMATION(#87)
SHAPE_REPRESENTATION_RELATIONSHIP()
);
#208=(
REPRESENTATION_RELATIONSHIP($,$,#13024,#13020)
REPRESENTATION_RELATIONSHIP_WITH_TRANSFORMATION(#88)
SHAPE_REPRESENTATION_RELATIONSHIP()
);
#209=(
REPRESENTATION_RELATIONSHIP($,$,#13024,#13020)
REPRESENTATION_RELATIONSHIP_WITH_TRANSFORMATION(#89)
SHAPE_REPRESENTATION_RELATIONSHIP()
);
#210=(
REPRESENTATION_RELATIONSHIP($,$,#13024,#13020)
REPRESENTATION_RELATIONSHIP_WITH_TRANSFORMATION(#90)
SHAPE_REPRESENTATION_RELATIONSHIP()
);
#211=(
REPRESENTATION_RELATIONSHIP($,$,#13028,#13020)
REPRESENTATION_RELATIONSHIP_WITH_TRANSFORMATION(#91)
SHAPE_REPRESENTATION_RELATIONSHIP()
);
#212=(
REPRESENTATION_RELATIONSHIP($,$,#13029,#13020)
REPRESENTATION_RELATIONSHIP_WITH_TRANSFORMATION(#92)
SHAPE_REPRESENTATION_RELATIONSHIP()
);
#213=(
REPRESENTATION_RELATIONSHIP($,$,#13028,#13020)
REPRESENTATION_RELATIONSHIP_WITH_TRANSFORMATION(#93)
SHAPE_REPRESENTATION_RELATIONSHIP()
);
#214=(
REPRESENTATION_RELATIONSHIP($,$,#13029,#13020)
REPRESENTATION_RELATIONSHIP_WITH_TRANSFORMATION(#94)
SHAPE_REPRESENTATION_RELATIONSHIP()
);
#215=(
REPRESENTATION_RELATIONSHIP($,$,#13028,#13020)
REPRESENTATION_RELATIONSHIP_WITH_TRANSFORMATION(#95)
SHAPE_REPRESENTATION_RELATIONSHIP()
);
#216=(
REPRESENTATION_RELATIONSHIP($,$,#13029,#13020)
REPRESENTATION_RELATIONSHIP_WITH_TRANSFORMATION(#96)
SHAPE_REPRESENTATION_RELATIONSHIP()
);
#217=(
REPRESENTATION_RELATIONSHIP($,$,#13028,#13020)
REPRESENTATION_RELATIONSHIP_WITH_TRANSFORMATION(#97)
SHAPE_REPRESENTATION_RELATIONSHIP()
);
#218=(
REPRESENTATION_RELATIONSHIP($,$,#13029,#13020)
REPRESENTATION_RELATIONSHIP_WITH_TRANSFORMATION(#98)
SHAPE_REPRESENTATION_RELATIONSHIP()
);
#219=(
REPRESENTATION_RELATIONSHIP($,$,#13028,#13020)
REPRESENTATION_RELATIONSHIP_WITH_TRANSFORMATION(#99)
SHAPE_REPRESENTATION_RELATIONSHIP()
);
#220=(
REPRESENTATION_RELATIONSHIP($,$,#13029,#13020)
REPRESENTATION_RELATIONSHIP_WITH_TRANSFORMATION(#100)
SHAPE_REPRESENTATION_RELATIONSHIP()
);
#221=(
REPRESENTATION_RELATIONSHIP($,$,#13028,#13020)
REPRESENTATION_RELATIONSHIP_WITH_TRANSFORMATION(#101)
SHAPE_REPRESENTATION_RELATIONSHIP()
);
#222=(
REPRESENTATION_RELATIONSHIP($,$,#13029,#13020)
REPRESENTATION_RELATIONSHIP_WITH_TRANSFORMATION(#102)
SHAPE_REPRESENTATION_RELATIONSHIP()
);
#223=(
REPRESENTATION_RELATIONSHIP($,$,#13028,#13020)
REPRESENTATION_RELATIONSHIP_WITH_TRANSFORMATION(#103)
SHAPE_REPRESENTATION_RELATIONSHIP()
);
#224=(
REPRESENTATION_RELATIONSHIP($,$,#13029,#13020)
REPRESENTATION_RELATIONSHIP_WITH_TRANSFORMATION(#104)
SHAPE_REPRESENTATION_RELATIONSHIP()
);
#225=(
REPRESENTATION_RELATIONSHIP($,$,#13028,#13020)
REPRESENTATION_RELATIONSHIP_WITH_TRANSFORMATION(#105)
SHAPE_REPRESENTATION_RELATIONSHIP()
);
#226=(
REPRESENTATION_RELATIONSHIP($,$,#13029,#13020)
REPRESENTATION_RELATIONSHIP_WITH_TRANSFORMATION(#106)
SHAPE_REPRESENTATION_RELATIONSHIP()
);
#227=(
REPRESENTATION_RELATIONSHIP($,$,#13028,#13020)
REPRESENTATION_RELATIONSHIP_WITH_TRANSFORMATION(#107)
SHAPE_REPRESENTATION_RELATIONSHIP()
);
#228=(
REPRESENTATION_RELATIONSHIP($,$,#13029,#13020)
REPRESENTATION_RELATIONSHIP_WITH_TRANSFORMATION(#108)
SHAPE_REPRESENTATION_RELATIONSHIP()
);
#229=(
REPRESENTATION_RELATIONSHIP($,$,#13028,#13020)
REPRESENTATION_RELATIONSHIP_WITH_TRANSFORMATION(#109)
SHAPE_REPRESENTATION_RELATIONSHIP()
);
#230=(
REPRESENTATION_RELATIONSHIP($,$,#13029,#13020)
REPRESENTATION_RELATIONSHIP_WITH_TRANSFORMATION(#110)
SHAPE_REPRESENTATION_RELATIONSHIP()
);
#231=(
REPRESENTATION_RELATIONSHIP($,$,#13028,#13020)
REPRESENTATION_RELATIONSHIP_WITH_TRANSFORMATION(#111)
SHAPE_REPRESENTATION_RELATIONSHIP()
);
#232=(
REPRESENTATION_RELATIONSHIP($,$,#13029,#13020)
REPRESENTATION_RELATIONSHIP_WITH_TRANSFORMATION(#112)
SHAPE_REPRESENTATION_RELATIONSHIP()
);
#233=(
REPRESENTATION_RELATIONSHIP($,$,#13028,#13020)
REPRESENTATION_RELATIONSHIP_WITH_TRANSFORMATION(#113)
SHAPE_REPRESENTATION_RELATIONSHIP()
);
#234=(
REPRESENTATION_RELATIONSHIP($,$,#13029,#13020)
REPRESENTATION_RELATIONSHIP_WITH_TRANSFORMATION(#114)
SHAPE_REPRESENTATION_RELATIONSHIP()
);
#235=(
REPRESENTATION_RELATIONSHIP($,$,#13028,#13020)
REPRESENTATION_RELATIONSHIP_WITH_TRANSFORMATION(#115)
SHAPE_REPRESENTATION_RELATIONSHIP()
);
#236=(
REPRESENTATION_RELATIONSHIP($,$,#13029,#13020)
REPRESENTATION_RELATIONSHIP_WITH_TRANSFORMATION(#116)
SHAPE_REPRESENTATION_RELATIONSHIP()
);
#237=(
REPRESENTATION_RELATIONSHIP($,$,#13028,#13020)
REPRESENTATION_RELATIONSHIP_WITH_TRANSFORMATION(#117)
SHAPE_REPRESENTATION_RELATIONSHIP()
);
#238=(
REPRESENTATION_RELATIONSHIP($,$,#13029,#13020)
REPRESENTATION_RELATIONSHIP_WITH_TRANSFORMATION(#118)
SHAPE_REPRESENTATION_RELATIONSHIP()
);
#239=(
REPRESENTATION_RELATIONSHIP($,$,#13028,#13020)
REPRESENTATION_RELATIONSHIP_WITH_TRANSFORMATION(#119)
SHAPE_REPRESENTATION_RELATIONSHIP()
);
#240=(
REPRESENTATION_RELATIONSHIP($,$,#13029,#13020)
REPRESENTATION_RELATIONSHIP_WITH_TRANSFORMATION(#120)
SHAPE_REPRESENTATION_RELATIONSHIP()
);
#241=(
REPRESENTATION_RELATIONSHIP($,$,#13028,#13020)
REPRESENTATION_RELATIONSHIP_WITH_TRANSFORMATION(#121)
SHAPE_REPRESENTATION_RELATIONSHIP()
);
#242=(
REPRESENTATION_RELATIONSHIP($,$,#13029,#13020)
REPRESENTATION_RELATIONSHIP_WITH_TRANSFORMATION(#122)
SHAPE_REPRESENTATION_RELATIONSHIP()
);
#243=(
REPRESENTATION_RELATIONSHIP($,$,#13030,#13020)
REPRESENTATION_RELATIONSHIP_WITH_TRANSFORMATION(#123)
SHAPE_REPRESENTATION_RELATIONSHIP()
);
#244=(
REPRESENTATION_RELATIONSHIP($,$,#13031,#13020)
REPRESENTATION_RELATIONSHIP_WITH_TRANSFORMATION(#124)
SHAPE_REPRESENTATION_RELATIONSHIP()
);
#245=(
REPRESENTATION_RELATIONSHIP($,$,#13032,#13020)
REPRESENTATION_RELATIONSHIP_WITH_TRANSFORMATION(#125)
SHAPE_REPRESENTATION_RELATIONSHIP()
);
#246=(
REPRESENTATION_RELATIONSHIP($,$,#13033,#13020)
REPRESENTATION_RELATIONSHIP_WITH_TRANSFORMATION(#126)
SHAPE_REPRESENTATION_RELATIONSHIP()
);
#247=(
REPRESENTATION_RELATIONSHIP($,$,#13032,#13020)
REPRESENTATION_RELATIONSHIP_WITH_TRANSFORMATION(#127)
SHAPE_REPRESENTATION_RELATIONSHIP()
);
#248=(
REPRESENTATION_RELATIONSHIP($,$,#13033,#13020)
REPRESENTATION_RELATIONSHIP_WITH_TRANSFORMATION(#128)
SHAPE_REPRESENTATION_RELATIONSHIP()
);
#249=(
REPRESENTATION_RELATIONSHIP($,$,#13000,#12999)
REPRESENTATION_RELATIONSHIP_WITH_TRANSFORMATION(#129)
SHAPE_REPRESENTATION_RELATIONSHIP()
);
#250=(
REPRESENTATION_RELATIONSHIP($,$,#13020,#12999)
REPRESENTATION_RELATIONSHIP_WITH_TRANSFORMATION(#130)
SHAPE_REPRESENTATION_RELATIONSHIP()
);
#251=CONTEXT_DEPENDENT_SHAPE_REPRESENTATION(#131,#12873);
#252=CONTEXT_DEPENDENT_SHAPE_REPRESENTATION(#132,#12874);
#253=CONTEXT_DEPENDENT_SHAPE_REPRESENTATION(#133,#12875);
#254=CONTEXT_DEPENDENT_SHAPE_REPRESENTATION(#134,#12877);
#255=CONTEXT_DEPENDENT_SHAPE_REPRESENTATION(#135,#12878);
#256=CONTEXT_DEPENDENT_SHAPE_REPRESENTATION(#136,#12879);
#257=CONTEXT_DEPENDENT_SHAPE_REPRESENTATION(#137,#12880);
#258=CONTEXT_DEPENDENT_SHAPE_REPRESENTATION(#138,#12881);
#259=CONTEXT_DEPENDENT_SHAPE_REPRESENTATION(#139,#12882);
#260=CONTEXT_DEPENDENT_SHAPE_REPRESENTATION(#140,#12883);
#261=CONTEXT_DEPENDENT_SHAPE_REPRESENTATION(#141,#12884);
#262=CONTEXT_DEPENDENT_SHAPE_REPRESENTATION(#142,#12885);
#263=CONTEXT_DEPENDENT_SHAPE_REPRESENTATION(#143,#12886);
#264=CONTEXT_DEPENDENT_SHAPE_REPRESENTATION(#144,#12887);
#265=CONTEXT_DEPENDENT_SHAPE_REPRESENTATION(#145,#12888);
#266=CONTEXT_DEPENDENT_SHAPE_REPRESENTATION(#146,#12889);
#267=CONTEXT_DEPENDENT_SHAPE_REPRESENTATION(#147,#12890);
#268=CONTEXT_DEPENDENT_SHAPE_REPRESENTATION(#148,#12891);
#269=CONTEXT_DEPENDENT_SHAPE_REPRESENTATION(#149,#12892);
#270=CONTEXT_DEPENDENT_SHAPE_REPRESENTATION(#150,#12893);
#271=CONTEXT_DEPENDENT_SHAPE_REPRESENTATION(#151,#12894);
#272=CONTEXT_DEPENDENT_SHAPE_REPRESENTATION(#152,#12895);
#273=CONTEXT_DEPENDENT_SHAPE_REPRESENTATION(#153,#12896);
#274=CONTEXT_DEPENDENT_SHAPE_REPRESENTATION(#154,#12897);
#275=CONTEXT_DEPENDENT_SHAPE_REPRESENTATION(#155,#12898);
#276=CONTEXT_DEPENDENT_SHAPE_REPRESENTATION(#156,#12899);
#277=CONTEXT_DEPENDENT_SHAPE_REPRESENTATION(#157,#12900);
#278=CONTEXT_DEPENDENT_SHAPE_REPRESENTATION(#158,#12901);
#279=CONTEXT_DEPENDENT_SHAPE_REPRESENTATION(#159,#12902);
#280=CONTEXT_DEPENDENT_SHAPE_REPRESENTATION(#160,#12903);
#281=CONTEXT_DEPENDENT_SHAPE_REPRESENTATION(#161,#12904);
#282=CONTEXT_DEPENDENT_SHAPE_REPRESENTATION(#162,#12905);
#283=CONTEXT_DEPENDENT_SHAPE_REPRESENTATION(#163,#12906);
#284=CONTEXT_DEPENDENT_SHAPE_REPRESENTATION(#164,#12907);
#285=CONTEXT_DEPENDENT_SHAPE_REPRESENTATION(#165,#12908);
#286=CONTEXT_DEPENDENT_SHAPE_REPRESENTATION(#166,#12909);
#287=CONTEXT_DEPENDENT_SHAPE_REPRESENTATION(#167,#12910);
#288=CONTEXT_DEPENDENT_SHAPE_REPRESENTATION(#168,#12911);
#289=CONTEXT_DEPENDENT_SHAPE_REPRESENTATION(#169,#12912);
#290=CONTEXT_DEPENDENT_SHAPE_REPRESENTATION(#170,#12913);
#291=CONTEXT_DEPENDENT_SHAPE_REPRESENTATION(#171,#12914);
#292=CONTEXT_DEPENDENT_SHAPE_REPRESENTATION(#172,#12915);
#293=CONTEXT_DEPENDENT_SHAPE_REPRESENTATION(#173,#12916);
#294=CONTEXT_DEPENDENT_SHAPE_REPRESENTATION(#174,#12917);
#295=CONTEXT_DEPENDENT_SHAPE_REPRESENTATION(#175,#12918);
#296=CONTEXT_DEPENDENT_SHAPE_REPRESENTATION(#176,#12919);
#297=CONTEXT_DEPENDENT_SHAPE_REPRESENTATION(#177,#12920);
#298=CONTEXT_DEPENDENT_SHAPE_REPRESENTATION(#178,#12921);
#299=CONTEXT_DEPENDENT_SHAPE_REPRESENTATION(#179,#12922);
#300=CONTEXT_DEPENDENT_SHAPE_REPRESENTATION(#180,#12923);
#301=CONTEXT_DEPENDENT_SHAPE_REPRESENTATION(#181,#12924);
#302=CONTEXT_DEPENDENT_SHAPE_REPRESENTATION(#182,#12925);
#303=CONTEXT_DEPENDENT_SHAPE_REPRESENTATION(#183,#12926);
#304=CONTEXT_DEPENDENT_SHAPE_REPRESENTATION(#184,#12927);
#305=CONTEXT_DEPENDENT_SHAPE_REPRESENTATION(#185,#12928);
#306=CONTEXT_DEPENDENT_SHAPE_REPRESENTATION(#186,#12929);
#307=CONTEXT_DEPENDENT_SHAPE_REPRESENTATION(#187,#12930);
#308=CONTEXT_DEPENDENT_SHAPE_REPRESENTATION(#188,#12931);
#309=CONTEXT_DEPENDENT_SHAPE_REPRESENTATION(#189,#12932);
#310=CONTEXT_DEPENDENT_SHAPE_REPRESENTATION(#190,#12933);
#311=CONTEXT_DEPENDENT_SHAPE_REPRESENTATION(#191,#12934);
#312=CONTEXT_DEPENDENT_SHAPE_REPRESENTATION(#192,#12935);
#313=CONTEXT_DEPENDENT_SHAPE_REPRESENTATION(#193,#12936);
#314=CONTEXT_DEPENDENT_SHAPE_REPRESENTATION(#194,#12937);
#315=CONTEXT_DEPENDENT_SHAPE_REPRESENTATION(#195,#12938);
#316=CONTEXT_DEPENDENT_SHAPE_REPRESENTATION(#196,#12939);
#317=CONTEXT_DEPENDENT_SHAPE_REPRESENTATION(#197,#12940);
#318=CONTEXT_DEPENDENT_SHAPE_REPRESENTATION(#198,#12941);
#319=CONTEXT_DEPENDENT_SHAPE_REPRESENTATION(#199,#12942);
#320=CONTEXT_DEPENDENT_SHAPE_REPRESENTATION(#200,#12943);
#321=CONTEXT_DEPENDENT_SHAPE_REPRESENTATION(#201,#12944);
#322=CONTEXT_DEPENDENT_SHAPE_REPRESENTATION(#202,#12945);
#323=CONTEXT_DEPENDENT_SHAPE_REPRESENTATION(#203,#12946);
#324=CONTEXT_DEPENDENT_SHAPE_REPRESENTATION(#204,#12952);
#325=CONTEXT_DEPENDENT_SHAPE_REPRESENTATION(#205,#12953);
#326=CONTEXT_DEPENDENT_SHAPE_REPRESENTATION(#206,#12954);
#327=CONTEXT_DEPENDENT_SHAPE_REPRESENTATION(#207,#12955);
#328=CONTEXT_DEPENDENT_SHAPE_REPRESENTATION(#208,#12956);
#329=CONTEXT_DEPENDENT_SHAPE_REPRESENTATION(#209,#12957);
#330=CONTEXT_DEPENDENT_SHAPE_REPRESENTATION(#210,#12958);
#331=CONTEXT_DEPENDENT_SHAPE_REPRESENTATION(#211,#12959);
#332=CONTEXT_DEPENDENT_SHAPE_REPRESENTATION(#212,#12960);
#333=CONTEXT_DEPENDENT_SHAPE_REPRESENTATION(#213,#12961);
#334=CONTEXT_DEPENDENT_SHAPE_REPRESENTATION(#214,#12962);
#335=CONTEXT_DEPENDENT_SHAPE_REPRESENTATION(#215,#12963);
#336=CONTEXT_DEPENDENT_SHAPE_REPRESENTATION(#216,#12964);
#337=CONTEXT_DEPENDENT_SHAPE_REPRESENTATION(#217,#12965);
#338=CONTEXT_DEPENDENT_SHAPE_REPRESENTATION(#218,#12966);
#339=CONTEXT_DEPENDENT_SHAPE_REPRESENTATION(#219,#12967);
#340=CONTEXT_DEPENDENT_SHAPE_REPRESENTATION(#220,#12968);
#341=CONTEXT_DEPENDENT_SHAPE_REPRESENTATION(#221,#12969);
#342=CONTEXT_DEPENDENT_SHAPE_REPRESENTATION(#222,#12970);
#343=CONTEXT_DEPENDENT_SHAPE_REPRESENTATION(#223,#12971);
#344=CONTEXT_DEPENDENT_SHAPE_REPRESENTATION(#224,#12972);
#345=CONTEXT_DEPENDENT_SHAPE_REPRESENTATION(#225,#12973);
#346=CONTEXT_DEPENDENT_SHAPE_REPRESENTATION(#226,#12974);
#347=CONTEXT_DEPENDENT_SHAPE_REPRESENTATION(#227,#12975);
#348=CONTEXT_DEPENDENT_SHAPE_REPRESENTATION(#228,#12976);
#349=CONTEXT_DEPENDENT_SHAPE_REPRESENTATION(#229,#12977);
#350=CONTEXT_DEPENDENT_SHAPE_REPRESENTATION(#230,#12978);
#351=CONTEXT_DEPENDENT_SHAPE_REPRESENTATION(#231,#12979);
#352=CONTEXT_DEPENDENT_SHAPE_REPRESENTATION(#232,#12980);
#353=CONTEXT_DEPENDENT_SHAPE_REPRESENTATION(#233,#12981);
#354=CONTEXT_DEPENDENT_SHAPE_REPRESENTATION(#234,#12982);
#355=CONTEXT_DEPENDENT_SHAPE_REPRESENTATION(#235,#12983);
#356=CONTEXT_DEPENDENT_SHAPE_REPRESENTATION(#236,#12984);
#357=CONTEXT_DEPENDENT_SHAPE_REPRESENTATION(#237,#12985);
#358=CONTEXT_DEPENDENT_SHAPE_REPRESENTATION(#238,#12986);
#359=CONTEXT_DEPENDENT_SHAPE_REPRESENTATION(#239,#12987);
#360=CONTEXT_DEPENDENT_SHAPE_REPRESENTATION(#240,#12988);
#361=CONTEXT_DEPENDENT_SHAPE_REPRESENTATION(#241,#12989);
#362=CONTEXT_DEPENDENT_SHAPE_REPRESENTATION(#242,#12990);
#363=CONTEXT_DEPENDENT_SHAPE_REPRESENTATION(#243,#12991);
#364=CONTEXT_DEPENDENT_SHAPE_REPRESENTATION(#244,#12992);
#365=CONTEXT_DEPENDENT_SHAPE_REPRESENTATION(#245,#12993);
#366=CONTEXT_DEPENDENT_SHAPE_REPRESENTATION(#246,#12994);
#367=CONTEXT_DEPENDENT_SHAPE_REPRESENTATION(#247,#12995);
#368=CONTEXT_DEPENDENT_SHAPE_REPRESENTATION(#248,#12996);
#369=CONTEXT_DEPENDENT_SHAPE_REPRESENTATION(#249,#12997);
#370=CONTEXT_DEPENDENT_SHAPE_REPRESENTATION(#250,#12998);
#371=NEXT_ASSEMBLY_USAGE_OCCURRENCE('Block:1','Block:1','Block:1',#13060,
#13061,'Block:1');
#372=NEXT_ASSEMBLY_USAGE_OCCURRENCE('End cap +:1','End cap +:1',
'End cap +:1',#13060,#13062,'End cap +:1');
#373=NEXT_ASSEMBLY_USAGE_OCCURRENCE('End cap:1','End cap:1','End cap:1',
#13060,#13063,'End cap:1');
#374=NEXT_ASSEMBLY_USAGE_OCCURRENCE('Rail adapter:1','Rail adapter:1',
'Rail adapter:1',#13036,#13037,'Rail adapter:1');
#375=NEXT_ASSEMBLY_USAGE_OCCURRENCE('Rail adapter (1):1',
'Rail adapter (1):1','Rail adapter (1):1',#13036,#13038,
'Rail adapter (1):1');
#376=NEXT_ASSEMBLY_USAGE_OCCURRENCE('End tie plate:1','End tie plate:1',
'End tie plate:1',#13036,#13039,'End tie plate:1');
#377=NEXT_ASSEMBLY_USAGE_OCCURRENCE('Cross foot:1','Cross foot:1',
'Cross foot:1',#13036,#13040,'Cross foot:1');
#378=NEXT_ASSEMBLY_USAGE_OCCURRENCE('Bonded foot pad:1',
'Bonded foot pad:1','Bonded foot pad:1',#13036,#13041,
'Bonded foot pad:1');
#379=NEXT_ASSEMBLY_USAGE_OCCURRENCE('Bonded foot pad (1):1',
'Bonded foot pad (1):1','Bonded foot pad (1):1',#13036,#13042,
'Bonded foot pad (1):1');
#380=NEXT_ASSEMBLY_USAGE_OCCURRENCE('End tie plate (1):1',
'End tie plate (1):1','End tie plate (1):1',#13036,#13043,
'End tie plate (1):1');
#381=NEXT_ASSEMBLY_USAGE_OCCURRENCE('Cross foot (1):1',
'Cross foot (1):1','Cross foot (1):1',#13036,#13044,'Cross foot (1):1');
#382=NEXT_ASSEMBLY_USAGE_OCCURRENCE('Bonded foot pad (2):1',
'Bonded foot pad (2):1','Bonded foot pad (2):1',#13036,#13045,
'Bonded foot pad (2):1');
#383=NEXT_ASSEMBLY_USAGE_OCCURRENCE('Bonded foot pad (3):1',
'Bonded foot pad (3):1','Bonded foot pad (3):1',#13036,#13046,
'Bonded foot pad (3):1');
#384=NEXT_ASSEMBLY_USAGE_OCCURRENCE('End stop beam:1','End stop beam:1',
'End stop beam:1',#13036,#13047,'End stop beam:1');
#385=NEXT_ASSEMBLY_USAGE_OCCURRENCE('Bonded stop pad:1',
'Bonded stop pad:1','Bonded stop pad:1',#13036,#13048,
'Bonded stop pad:1');
#386=NEXT_ASSEMBLY_USAGE_OCCURRENCE('End stop beam (1):1',
'End stop beam (1):1','End stop beam (1):1',#13036,#13049,
'End stop beam (1):1');
#387=NEXT_ASSEMBLY_USAGE_OCCURRENCE('Bonded stop pad (1):1',
'Bonded stop pad (1):1','Bonded stop pad (1):1',#13036,#13050,
'Bonded stop pad (1):1');
#388=NEXT_ASSEMBLY_USAGE_OCCURRENCE(
'Slotted Extrusion - 20 x 20 x 400 mm:2',
'Slotted Extrusion - 20 x 20 x 400 mm:2',
'Slotted Extrusion - 20 x 20 x 400 mm:2',#13036,#13051,
'Slotted Extrusion - 20 x 20 x 400 mm:2');
#389=NEXT_ASSEMBLY_USAGE_OCCURRENCE('Captive slot nut:2',
'Captive slot nut:2','Captive slot nut:2',#13036,#13054,
'Captive slot nut:2');
#390=NEXT_ASSEMBLY_USAGE_OCCURRENCE('Flat Washer - M5:2',
'Flat Washer - M5:2','Flat Washer - M5:2',#13036,#13064,
'Flat Washer - M5:2');
#391=NEXT_ASSEMBLY_USAGE_OCCURRENCE('M5x14 Cap Screw:2',
'M5x14 Cap Screw:2','M5x14 Cap Screw:2',#13036,#13055,
'M5x14 Cap Screw:2');
#392=NEXT_ASSEMBLY_USAGE_OCCURRENCE('Captive slot nut:3',
'Captive slot nut:3','Captive slot nut:3',#13036,#13054,
'Captive slot nut:3');
#393=NEXT_ASSEMBLY_USAGE_OCCURRENCE('Flat Washer - M5:3',
'Flat Washer - M5:3','Flat Washer - M5:3',#13036,#13064,
'Flat Washer - M5:3');
#394=NEXT_ASSEMBLY_USAGE_OCCURRENCE('M5x14 Cap Screw:3',
'M5x14 Cap Screw:3','M5x14 Cap Screw:3',#13036,#13055,
'M5x14 Cap Screw:3');
#395=NEXT_ASSEMBLY_USAGE_OCCURRENCE(
'Linear Guide Rail - 15 mm, 220 mm Long:2',
'Linear Guide Rail - 15 mm, 220 mm Long:2',
'Linear Guide Rail - 15 mm, 220 mm Long:2',#13036,#13052,
'Linear Guide Rail - 15 mm, 220 mm Long:2');
#396=NEXT_ASSEMBLY_USAGE_OCCURRENCE('Cap Screw - M4x16:2',
'Cap Screw - M4x16:2','Cap Screw - M4x16:2',#13036,#13053,
'Cap Screw - M4x16:2');
#397=NEXT_ASSEMBLY_USAGE_OCCURRENCE('Cap Screw - M4x16:3',
'Cap Screw - M4x16:3','Cap Screw - M4x16:3',#13036,#13053,
'Cap Screw - M4x16:3');
#398=NEXT_ASSEMBLY_USAGE_OCCURRENCE('Cap Screw - M4x16:4',
'Cap Screw - M4x16:4','Cap Screw - M4x16:4',#13036,#13053,
'Cap Screw - M4x16:4');
#399=NEXT_ASSEMBLY_USAGE_OCCURRENCE('Cap Screw - M4x16:5',
'Cap Screw - M4x16:5','Cap Screw - M4x16:5',#13036,#13053,
'Cap Screw - M4x16:5');
#400=NEXT_ASSEMBLY_USAGE_OCCURRENCE(
'Slotted Extrusion - 20 x 20 x 400 mm:3',
'Slotted Extrusion - 20 x 20 x 400 mm:3',
'Slotted Extrusion - 20 x 20 x 400 mm:3',#13036,#13051,
'Slotted Extrusion - 20 x 20 x 400 mm:3');
#401=NEXT_ASSEMBLY_USAGE_OCCURRENCE('Captive slot nut:4',
'Captive slot nut:4','Captive slot nut:4',#13036,#13054,
'Captive slot nut:4');
#402=NEXT_ASSEMBLY_USAGE_OCCURRENCE('Flat Washer - M5:4',
'Flat Washer - M5:4','Flat Washer - M5:4',#13036,#13064,
'Flat Washer - M5:4');
#403=NEXT_ASSEMBLY_USAGE_OCCURRENCE('M5x14 Cap Screw:4',
'M5x14 Cap Screw:4','M5x14 Cap Screw:4',#13036,#13055,
'M5x14 Cap Screw:4');
#404=NEXT_ASSEMBLY_USAGE_OCCURRENCE('Captive slot nut:5',
'Captive slot nut:5','Captive slot nut:5',#13036,#13054,
'Captive slot nut:5');
#405=NEXT_ASSEMBLY_USAGE_OCCURRENCE('Flat Washer - M5:5',
'Flat Washer - M5:5','Flat Washer - M5:5',#13036,#13064,
'Flat Washer - M5:5');
#406=NEXT_ASSEMBLY_USAGE_OCCURRENCE('M5x14 Cap Screw:5',
'M5x14 Cap Screw:5','M5x14 Cap Screw:5',#13036,#13055,
'M5x14 Cap Screw:5');
#407=NEXT_ASSEMBLY_USAGE_OCCURRENCE(
'Linear Guide Rail - 15 mm, 220 mm Long:3',
'Linear Guide Rail - 15 mm, 220 mm Long:3',
'Linear Guide Rail - 15 mm, 220 mm Long:3',#13036,#13052,
'Linear Guide Rail - 15 mm, 220 mm Long:3');
#408=NEXT_ASSEMBLY_USAGE_OCCURRENCE('Cap Screw - M4x16:6',
'Cap Screw - M4x16:6','Cap Screw - M4x16:6',#13036,#13053,
'Cap Screw - M4x16:6');
#409=NEXT_ASSEMBLY_USAGE_OCCURRENCE('Cap Screw - M4x16:7',
'Cap Screw - M4x16:7','Cap Screw - M4x16:7',#13036,#13053,
'Cap Screw - M4x16:7');
#410=NEXT_ASSEMBLY_USAGE_OCCURRENCE('Cap Screw - M4x16:8',
'Cap Screw - M4x16:8','Cap Screw - M4x16:8',#13036,#13053,
'Cap Screw - M4x16:8');
#411=NEXT_ASSEMBLY_USAGE_OCCURRENCE('Cap Screw - M4x16:9',
'Cap Screw - M4x16:9','Cap Screw - M4x16:9',#13036,#13053,
'Cap Screw - M4x16:9');
#412=NEXT_ASSEMBLY_USAGE_OCCURRENCE('Captive slot nut:6',
'Captive slot nut:6','Captive slot nut:6',#13036,#13054,
'Captive slot nut:6');
#413=NEXT_ASSEMBLY_USAGE_OCCURRENCE('Flat Washer - M5:6',
'Flat Washer - M5:6','Flat Washer - M5:6',#13036,#13064,
'Flat Washer - M5:6');
#414=NEXT_ASSEMBLY_USAGE_OCCURRENCE('M5x14 Cap Screw:6',
'M5x14 Cap Screw:6','M5x14 Cap Screw:6',#13036,#13055,
'M5x14 Cap Screw:6');
#415=NEXT_ASSEMBLY_USAGE_OCCURRENCE('Captive slot nut:7',
'Captive slot nut:7','Captive slot nut:7',#13036,#13054,
'Captive slot nut:7');
#416=NEXT_ASSEMBLY_USAGE_OCCURRENCE('Flat Washer - M5:7',
'Flat Washer - M5:7','Flat Washer - M5:7',#13036,#13064,
'Flat Washer - M5:7');
#417=NEXT_ASSEMBLY_USAGE_OCCURRENCE('M5x14 Cap Screw:7',
'M5x14 Cap Screw:7','M5x14 Cap Screw:7',#13036,#13055,
'M5x14 Cap Screw:7');
#418=NEXT_ASSEMBLY_USAGE_OCCURRENCE('Captive slot nut:8',
'Captive slot nut:8','Captive slot nut:8',#13036,#13054,
'Captive slot nut:8');
#419=NEXT_ASSEMBLY_USAGE_OCCURRENCE('Flat Washer - M5:8',
'Flat Washer - M5:8','Flat Washer - M5:8',#13036,#13064,
'Flat Washer - M5:8');
#420=NEXT_ASSEMBLY_USAGE_OCCURRENCE('M5x14 Cap Screw:8',
'M5x14 Cap Screw:8','M5x14 Cap Screw:8',#13036,#13055,
'M5x14 Cap Screw:8');
#421=NEXT_ASSEMBLY_USAGE_OCCURRENCE('Captive slot nut:9',
'Captive slot nut:9','Captive slot nut:9',#13036,#13054,
'Captive slot nut:9');
#422=NEXT_ASSEMBLY_USAGE_OCCURRENCE('Flat Washer - M5:9',
'Flat Washer - M5:9','Flat Washer - M5:9',#13036,#13064,
'Flat Washer - M5:9');
#423=NEXT_ASSEMBLY_USAGE_OCCURRENCE('M5x14 Cap Screw:9',
'M5x14 Cap Screw:9','M5x14 Cap Screw:9',#13036,#13055,
'M5x14 Cap Screw:9');
#424=NEXT_ASSEMBLY_USAGE_OCCURRENCE('Captive slot nut:10',
'Captive slot nut:10','Captive slot nut:10',#13036,#13054,
'Captive slot nut:10');
#425=NEXT_ASSEMBLY_USAGE_OCCURRENCE('Flat Washer - M5:10',
'Flat Washer - M5:10','Flat Washer - M5:10',#13036,#13064,
'Flat Washer - M5:10');
#426=NEXT_ASSEMBLY_USAGE_OCCURRENCE('M5x14 Cap Screw:10',
'M5x14 Cap Screw:10','M5x14 Cap Screw:10',#13036,#13055,
'M5x14 Cap Screw:10');
#427=NEXT_ASSEMBLY_USAGE_OCCURRENCE('Captive slot nut:11',
'Captive slot nut:11','Captive slot nut:11',#13036,#13054,
'Captive slot nut:11');
#428=NEXT_ASSEMBLY_USAGE_OCCURRENCE('Flat Washer - M5:11',
'Flat Washer - M5:11','Flat Washer - M5:11',#13036,#13064,
'Flat Washer - M5:11');
#429=NEXT_ASSEMBLY_USAGE_OCCURRENCE('M5x14 Cap Screw:11',
'M5x14 Cap Screw:11','M5x14 Cap Screw:11',#13036,#13055,
'M5x14 Cap Screw:11');
#430=NEXT_ASSEMBLY_USAGE_OCCURRENCE('Captive slot nut:12',
'Captive slot nut:12','Captive slot nut:12',#13036,#13054,
'Captive slot nut:12');
#431=NEXT_ASSEMBLY_USAGE_OCCURRENCE('Flat Washer - M5:12',
'Flat Washer - M5:12','Flat Washer - M5:12',#13036,#13064,
'Flat Washer - M5:12');
#432=NEXT_ASSEMBLY_USAGE_OCCURRENCE('M5x14 Cap Screw:12',
'M5x14 Cap Screw:12','M5x14 Cap Screw:12',#13036,#13055,
'M5x14 Cap Screw:12');
#433=NEXT_ASSEMBLY_USAGE_OCCURRENCE('Captive slot nut:13',
'Captive slot nut:13','Captive slot nut:13',#13036,#13054,
'Captive slot nut:13');
#434=NEXT_ASSEMBLY_USAGE_OCCURRENCE('Flat Washer - M5:13',
'Flat Washer - M5:13','Flat Washer - M5:13',#13036,#13064,
'Flat Washer - M5:13');
#435=NEXT_ASSEMBLY_USAGE_OCCURRENCE('M5x14 Cap Screw:13',
'M5x14 Cap Screw:13','M5x14 Cap Screw:13',#13036,#13055,
'M5x14 Cap Screw:13');
#436=NEXT_ASSEMBLY_USAGE_OCCURRENCE('Captive slot nut:14',
'Captive slot nut:14','Captive slot nut:14',#13036,#13054,
'Captive slot nut:14');
#437=NEXT_ASSEMBLY_USAGE_OCCURRENCE('M5x14 Cap Screw:14',
'M5x14 Cap Screw:14','M5x14 Cap Screw:14',#13036,#13055,
'M5x14 Cap Screw:14');
#438=NEXT_ASSEMBLY_USAGE_OCCURRENCE('Captive slot nut:15',
'Captive slot nut:15','Captive slot nut:15',#13036,#13054,
'Captive slot nut:15');
#439=NEXT_ASSEMBLY_USAGE_OCCURRENCE('M5x14 Cap Screw:15',
'M5x14 Cap Screw:15','M5x14 Cap Screw:15',#13036,#13055,
'M5x14 Cap Screw:15');
#440=NEXT_ASSEMBLY_USAGE_OCCURRENCE('Captive slot nut:16',
'Captive slot nut:16','Captive slot nut:16',#13036,#13054,
'Captive slot nut:16');
#441=NEXT_ASSEMBLY_USAGE_OCCURRENCE('M5x14 Cap Screw:16',
'M5x14 Cap Screw:16','M5x14 Cap Screw:16',#13036,#13055,
'M5x14 Cap Screw:16');
#442=NEXT_ASSEMBLY_USAGE_OCCURRENCE('Captive slot nut:17',
'Captive slot nut:17','Captive slot nut:17',#13036,#13054,
'Captive slot nut:17');
#443=NEXT_ASSEMBLY_USAGE_OCCURRENCE('M5x14 Cap Screw:17',
'M5x14 Cap Screw:17','M5x14 Cap Screw:17',#13036,#13055,
'M5x14 Cap Screw:17');
#444=NEXT_ASSEMBLY_USAGE_OCCURRENCE('Bridge table:1','Bridge table:1',
'Bridge table:1',#13056,#13057,'Bridge table:1');
#445=NEXT_ASSEMBLY_USAGE_OCCURRENCE('Manual grip:1','Manual grip:1',
'Manual grip:1',#13056,#13058,'Manual grip:1');
#446=NEXT_ASSEMBLY_USAGE_OCCURRENCE('Cable bracket:1','Cable bracket:1',
'Cable bracket:1',#13056,#13059,'Cable bracket:1');
#447=NEXT_ASSEMBLY_USAGE_OCCURRENCE(
'Flanged Linear Guide Carriage - 15 mm:2',
'Flanged Linear Guide Carriage - 15 mm:2',
'Flanged Linear Guide Carriage - 15 mm:2',#13056,#13060,
'Flanged Linear Guide Carriage - 15 mm:2');
#448=NEXT_ASSEMBLY_USAGE_OCCURRENCE(
'Flanged Linear Guide Carriage - 15 mm:3',
'Flanged Linear Guide Carriage - 15 mm:3',
'Flanged Linear Guide Carriage - 15 mm:3',#13056,#13060,
'Flanged Linear Guide Carriage - 15 mm:3');
#449=NEXT_ASSEMBLY_USAGE_OCCURRENCE(
'Flanged Linear Guide Carriage - 15 mm:4',
'Flanged Linear Guide Carriage - 15 mm:4',
'Flanged Linear Guide Carriage - 15 mm:4',#13056,#13060,
'Flanged Linear Guide Carriage - 15 mm:4');
#450=NEXT_ASSEMBLY_USAGE_OCCURRENCE(
'Flanged Linear Guide Carriage - 15 mm:5',
'Flanged Linear Guide Carriage - 15 mm:5',
'Flanged Linear Guide Carriage - 15 mm:5',#13056,#13060,
'Flanged Linear Guide Carriage - 15 mm:5');
#451=NEXT_ASSEMBLY_USAGE_OCCURRENCE('Flat Washer - M5:14',
'Flat Washer - M5:14','Flat Washer - M5:14',#13056,#13064,
'Flat Washer - M5:14');
#452=NEXT_ASSEMBLY_USAGE_OCCURRENCE('Cap Screw - M5x20:2',
'Cap Screw - M5x20:2','Cap Screw - M5x20:2',#13056,#13065,
'Cap Screw - M5x20:2');
#453=NEXT_ASSEMBLY_USAGE_OCCURRENCE('Flat Washer - M5:15',
'Flat Washer - M5:15','Flat Washer - M5:15',#13056,#13064,
'Flat Washer - M5:15');
#454=NEXT_ASSEMBLY_USAGE_OCCURRENCE('Cap Screw - M5x20:3',
'Cap Screw - M5x20:3','Cap Screw - M5x20:3',#13056,#13065,
'Cap Screw - M5x20:3');
#455=NEXT_ASSEMBLY_USAGE_OCCURRENCE('Flat Washer - M5:16',
'Flat Washer - M5:16','Flat Washer - M5:16',#13056,#13064,
'Flat Washer - M5:16');
#456=NEXT_ASSEMBLY_USAGE_OCCURRENCE('Cap Screw - M5x20:4',
'Cap Screw - M5x20:4','Cap Screw - M5x20:4',#13056,#13065,
'Cap Screw - M5x20:4');
#457=NEXT_ASSEMBLY_USAGE_OCCURRENCE('Flat Washer - M5:17',
'Flat Washer - M5:17','Flat Washer - M5:17',#13056,#13064,
'Flat Washer - M5:17');
#458=NEXT_ASSEMBLY_USAGE_OCCURRENCE('Cap Screw - M5x20:5',
'Cap Screw - M5x20:5','Cap Screw - M5x20:5',#13056,#13065,
'Cap Screw - M5x20:5');
#459=NEXT_ASSEMBLY_USAGE_OCCURRENCE('Flat Washer - M5:18',
'Flat Washer - M5:18','Flat Washer - M5:18',#13056,#13064,
'Flat Washer - M5:18');
#460=NEXT_ASSEMBLY_USAGE_OCCURRENCE('Cap Screw - M5x20:6',
'Cap Screw - M5x20:6','Cap Screw - M5x20:6',#13056,#13065,
'Cap Screw - M5x20:6');
#461=NEXT_ASSEMBLY_USAGE_OCCURRENCE('Flat Washer - M5:19',
'Flat Washer - M5:19','Flat Washer - M5:19',#13056,#13064,
'Flat Washer - M5:19');
#462=NEXT_ASSEMBLY_USAGE_OCCURRENCE('Cap Screw - M5x20:7',
'Cap Screw - M5x20:7','Cap Screw - M5x20:7',#13056,#13065,
'Cap Screw - M5x20:7');
#463=NEXT_ASSEMBLY_USAGE_OCCURRENCE('Flat Washer - M5:20',
'Flat Washer - M5:20','Flat Washer - M5:20',#13056,#13064,
'Flat Washer - M5:20');
#464=NEXT_ASSEMBLY_USAGE_OCCURRENCE('Cap Screw - M5x20:8',
'Cap Screw - M5x20:8','Cap Screw - M5x20:8',#13056,#13065,
'Cap Screw - M5x20:8');
#465=NEXT_ASSEMBLY_USAGE_OCCURRENCE('Flat Washer - M5:21',
'Flat Washer - M5:21','Flat Washer - M5:21',#13056,#13064,
'Flat Washer - M5:21');
#466=NEXT_ASSEMBLY_USAGE_OCCURRENCE('Cap Screw - M5x20:9',
'Cap Screw - M5x20:9','Cap Screw - M5x20:9',#13056,#13065,
'Cap Screw - M5x20:9');
#467=NEXT_ASSEMBLY_USAGE_OCCURRENCE('Flat Washer - M5:22',
'Flat Washer - M5:22','Flat Washer - M5:22',#13056,#13064,
'Flat Washer - M5:22');
#468=NEXT_ASSEMBLY_USAGE_OCCURRENCE('Cap Screw - M5x20:10',
'Cap Screw - M5x20:10','Cap Screw - M5x20:10',#13056,#13065,
'Cap Screw - M5x20:10');
#469=NEXT_ASSEMBLY_USAGE_OCCURRENCE('Flat Washer - M5:23',
'Flat Washer - M5:23','Flat Washer - M5:23',#13056,#13064,
'Flat Washer - M5:23');
#470=NEXT_ASSEMBLY_USAGE_OCCURRENCE('Cap Screw - M5x20:11',
'Cap Screw - M5x20:11','Cap Screw - M5x20:11',#13056,#13065,
'Cap Screw - M5x20:11');
#471=NEXT_ASSEMBLY_USAGE_OCCURRENCE('Flat Washer - M5:24',
'Flat Washer - M5:24','Flat Washer - M5:24',#13056,#13064,
'Flat Washer - M5:24');
#472=NEXT_ASSEMBLY_USAGE_OCCURRENCE('Cap Screw - M5x20:12',
'Cap Screw - M5x20:12','Cap Screw - M5x20:12',#13056,#13065,
'Cap Screw - M5x20:12');
#473=NEXT_ASSEMBLY_USAGE_OCCURRENCE('Flat Washer - M5:25',
'Flat Washer - M5:25','Flat Washer - M5:25',#13056,#13064,
'Flat Washer - M5:25');
#474=NEXT_ASSEMBLY_USAGE_OCCURRENCE('Cap Screw - M5x20:13',
'Cap Screw - M5x20:13','Cap Screw - M5x20:13',#13056,#13065,
'Cap Screw - M5x20:13');
#475=NEXT_ASSEMBLY_USAGE_OCCURRENCE('Flat Washer - M5:26',
'Flat Washer - M5:26','Flat Washer - M5:26',#13056,#13064,
'Flat Washer - M5:26');
#476=NEXT_ASSEMBLY_USAGE_OCCURRENCE('Cap Screw - M5x20:14',
'Cap Screw - M5x20:14','Cap Screw - M5x20:14',#13056,#13065,
'Cap Screw - M5x20:14');
#477=NEXT_ASSEMBLY_USAGE_OCCURRENCE('Flat Washer - M5:27',
'Flat Washer - M5:27','Flat Washer - M5:27',#13056,#13064,
'Flat Washer - M5:27');
#478=NEXT_ASSEMBLY_USAGE_OCCURRENCE('Cap Screw - M5x20:15',
'Cap Screw - M5x20:15','Cap Screw - M5x20:15',#13056,#13065,
'Cap Screw - M5x20:15');
#479=NEXT_ASSEMBLY_USAGE_OCCURRENCE('Flat Washer - M5:28',
'Flat Washer - M5:28','Flat Washer - M5:28',#13056,#13064,
'Flat Washer - M5:28');
#480=NEXT_ASSEMBLY_USAGE_OCCURRENCE('Cap Screw - M5x20:16',
'Cap Screw - M5x20:16','Cap Screw - M5x20:16',#13056,#13065,
'Cap Screw - M5x20:16');
#481=NEXT_ASSEMBLY_USAGE_OCCURRENCE('Flat Washer - M5:29',
'Flat Washer - M5:29','Flat Washer - M5:29',#13056,#13064,
'Flat Washer - M5:29');
#482=NEXT_ASSEMBLY_USAGE_OCCURRENCE('Cap Screw - M5x20:17',
'Cap Screw - M5x20:17','Cap Screw - M5x20:17',#13056,#13065,
'Cap Screw - M5x20:17');
#483=NEXT_ASSEMBLY_USAGE_OCCURRENCE('Flat Washer - M6:2',
'Flat Washer - M6:2','Flat Washer - M6:2',#13056,#13066,
'Flat Washer - M6:2');
#484=NEXT_ASSEMBLY_USAGE_OCCURRENCE('Cap Screw - M6x25:2',
'Cap Screw - M6x25:2','Cap Screw - M6x25:2',#13056,#13067,
'Cap Screw - M6x25:2');
#485=NEXT_ASSEMBLY_USAGE_OCCURRENCE('Flat Washer - M4:2',
'Flat Washer - M4:2','Flat Washer - M4:2',#13056,#13068,
'Flat Washer - M4:2');
#486=NEXT_ASSEMBLY_USAGE_OCCURRENCE('M4x10 Cap Screw:2',
'M4x10 Cap Screw:2','M4x10 Cap Screw:2',#13056,#13069,
'M4x10 Cap Screw:2');
#487=NEXT_ASSEMBLY_USAGE_OCCURRENCE('Flat Washer - M4:3',
'Flat Washer - M4:3','Flat Washer - M4:3',#13056,#13068,
'Flat Washer - M4:3');
#488=NEXT_ASSEMBLY_USAGE_OCCURRENCE('M4x10 Cap Screw:3',
'M4x10 Cap Screw:3','M4x10 Cap Screw:3',#13056,#13069,
'M4x10 Cap Screw:3');
#489=NEXT_ASSEMBLY_USAGE_OCCURRENCE('Rail frame:1','Rail frame:1',
'Rail frame:1',#13035,#13036,'Rail frame:1');
#490=NEXT_ASSEMBLY_USAGE_OCCURRENCE('Moving bridge:1','Moving bridge:1',
'Moving bridge:1',#13035,#13056,'Moving bridge:1');
#491=ELLIPSE('',#8075,0.299389011154384,0.2117);
#492=ELLIPSE('',#8079,0.299389011154384,0.2117);
#493=ORIENTED_CLOSED_SHELL('',*,#7380,.F.);
#494=ORIENTED_CLOSED_SHELL('',*,#7382,.F.);
#495=ORIENTED_CLOSED_SHELL('',*,#7392,.F.);
#496=ORIENTED_CLOSED_SHELL('',*,#7395,.F.);
#497=ORIENTED_CLOSED_SHELL('',*,#7397,.F.);
#498=CONICAL_SURFACE('',#8041,0.325,0.785398163397448);
#499=CONICAL_SURFACE('',#8045,0.335,0.785398163397448);
#500=CONICAL_SURFACE('',#8049,0.21,0.463647609000806);
#501=CONICAL_SURFACE('',#8053,0.18,0.785398163397448);
#502=CONICAL_SURFACE('',#8098,0.4,0.785398163397448);
#503=CONICAL_SURFACE('',#8102,0.41,0.785398163397448);
#504=CONICAL_SURFACE('',#8106,0.26,0.463647609000806);
#505=CONICAL_SURFACE('',#8264,0.275,0.785398163397449);
#506=CONICAL_SURFACE('',#8347,0.4,0.785398163397448);
#507=CONICAL_SURFACE('',#8351,0.41,0.785398163397448);
#508=CONICAL_SURFACE('',#8355,0.26,0.463647609000806);
#509=CONICAL_SURFACE('',#8359,0.225,0.785398163397448);
#510=CONICAL_SURFACE('',#8382,0.475,0.785398163397449);
#511=CONICAL_SURFACE('',#8386,0.485,0.785398163397448);
#512=CONICAL_SURFACE('',#8390,0.31,0.463647609000806);
#513=CONICAL_SURFACE('',#8394,0.27,0.785398163397448);
#514=CONICAL_SURFACE('',#8406,0.225,0.785398163397448);
#515=CONICAL_SURFACE('',#8429,0.325,0.785398163397448);
#516=CONICAL_SURFACE('',#8433,0.335,0.785398163397448);
#517=CONICAL_SURFACE('',#8437,0.21,0.463647609000806);
#518=BREP_WITH_VOIDS('Body1',#7379,(#493));
#519=BREP_WITH_VOIDS('Body1',#7383,(#494));
#520=BREP_WITH_VOIDS('Body1',#7391,(#495));
#521=BREP_WITH_VOIDS('Body1',#7394,(#496));
#522=BREP_WITH_VOIDS('Body1',#7398,(#497));
#523=SHAPE_REPRESENTATION_RELATIONSHIP('SRR','None',#13001,#554);
#524=SHAPE_REPRESENTATION_RELATIONSHIP('SRR','None',#13002,#555);
#525=SHAPE_REPRESENTATION_RELATIONSHIP('SRR','None',#13003,#556);
#526=SHAPE_REPRESENTATION_RELATIONSHIP('SRR','None',#13004,#557);
#527=SHAPE_REPRESENTATION_RELATIONSHIP('SRR','None',#13005,#558);
#528=SHAPE_REPRESENTATION_RELATIONSHIP('SRR','None',#13006,#559);
#529=SHAPE_REPRESENTATION_RELATIONSHIP('SRR','None',#13007,#560);
#530=SHAPE_REPRESENTATION_RELATIONSHIP('SRR','None',#13008,#561);
#531=SHAPE_REPRESENTATION_RELATIONSHIP('SRR','None',#13009,#562);
#532=SHAPE_REPRESENTATION_RELATIONSHIP('SRR','None',#13010,#563);
#533=SHAPE_REPRESENTATION_RELATIONSHIP('SRR','None',#13011,#564);
#534=SHAPE_REPRESENTATION_RELATIONSHIP('SRR','None',#13012,#565);
#535=SHAPE_REPRESENTATION_RELATIONSHIP('SRR','None',#13013,#566);
#536=SHAPE_REPRESENTATION_RELATIONSHIP('SRR','None',#13014,#567);
#537=SHAPE_REPRESENTATION_RELATIONSHIP('SRR','None',#13015,#568);
#538=SHAPE_REPRESENTATION_RELATIONSHIP('SRR','None',#13016,#569);
#539=SHAPE_REPRESENTATION_RELATIONSHIP('SRR','None',#13017,#570);
#540=SHAPE_REPRESENTATION_RELATIONSHIP('SRR','None',#13018,#571);
#541=SHAPE_REPRESENTATION_RELATIONSHIP('SRR','None',#13019,#572);
#542=SHAPE_REPRESENTATION_RELATIONSHIP('SRR','None',#13021,#573);
#543=SHAPE_REPRESENTATION_RELATIONSHIP('SRR','None',#13022,#574);
#544=SHAPE_REPRESENTATION_RELATIONSHIP('SRR','None',#13023,#575);
#545=SHAPE_REPRESENTATION_RELATIONSHIP('SRR','None',#13025,#576);
#546=SHAPE_REPRESENTATION_RELATIONSHIP('SRR','None',#13026,#577);
#547=SHAPE_REPRESENTATION_RELATIONSHIP('SRR','None',#13027,#578);
#548=SHAPE_REPRESENTATION_RELATIONSHIP('SRR','None',#13028,#579);
#549=SHAPE_REPRESENTATION_RELATIONSHIP('SRR','None',#13029,#580);
#550=SHAPE_REPRESENTATION_RELATIONSHIP('SRR','None',#13030,#581);
#551=SHAPE_REPRESENTATION_RELATIONSHIP('SRR','None',#13031,#582);
#552=SHAPE_REPRESENTATION_RELATIONSHIP('SRR','None',#13032,#583);
#553=SHAPE_REPRESENTATION_RELATIONSHIP('SRR','None',#13033,#584);
#554=ADVANCED_BREP_SHAPE_REPRESENTATION('',(#616),#12771);
#555=ADVANCED_BREP_SHAPE_REPRESENTATION('',(#617),#12772);
#556=ADVANCED_BREP_SHAPE_REPRESENTATION('',(#618),#12773);
#557=ADVANCED_BREP_SHAPE_REPRESENTATION('',(#619),#12774);
#558=ADVANCED_BREP_SHAPE_REPRESENTATION('',(#620),#12775);
#559=ADVANCED_BREP_SHAPE_REPRESENTATION('',(#621),#12776);
#560=ADVANCED_BREP_SHAPE_REPRESENTATION('',(#622),#12777);
#561=ADVANCED_BREP_SHAPE_REPRESENTATION('',(#623),#12778);
#562=ADVANCED_BREP_SHAPE_REPRESENTATION('',(#624),#12779);
#563=ADVANCED_BREP_SHAPE_REPRESENTATION('',(#625),#12780);
#564=ADVANCED_BREP_SHAPE_REPRESENTATION('',(#626),#12781);
#565=ADVANCED_BREP_SHAPE_REPRESENTATION('',(#627),#12782);
#566=ADVANCED_BREP_SHAPE_REPRESENTATION('',(#628),#12783);
#567=ADVANCED_BREP_SHAPE_REPRESENTATION('',(#629),#12784);
#568=ADVANCED_BREP_SHAPE_REPRESENTATION('',(#630),#12785);
#569=ADVANCED_BREP_SHAPE_REPRESENTATION('',(#631),#12786);
#570=ADVANCED_BREP_SHAPE_REPRESENTATION('',(#518),#12787);
#571=ADVANCED_BREP_SHAPE_REPRESENTATION('',(#632),#12788);
#572=ADVANCED_BREP_SHAPE_REPRESENTATION('',(#519),#12789);
#573=ADVANCED_BREP_SHAPE_REPRESENTATION('',(#633),#12791);
#574=ADVANCED_BREP_SHAPE_REPRESENTATION('',(#634),#12792);
#575=ADVANCED_BREP_SHAPE_REPRESENTATION('',(#635),#12793);
#576=ADVANCED_BREP_SHAPE_REPRESENTATION('',(#636),#12795);
#577=ADVANCED_BREP_SHAPE_REPRESENTATION('',(#637),#12796);
#578=ADVANCED_BREP_SHAPE_REPRESENTATION('',(#638),#12797);
#579=ADVANCED_BREP_SHAPE_REPRESENTATION('',(#639),#12798);
#580=ADVANCED_BREP_SHAPE_REPRESENTATION('',(#520),#12799);
#581=ADVANCED_BREP_SHAPE_REPRESENTATION('',(#640),#12800);
#582=ADVANCED_BREP_SHAPE_REPRESENTATION('',(#521),#12801);
#583=ADVANCED_BREP_SHAPE_REPRESENTATION('',(#641),#12802);
#584=ADVANCED_BREP_SHAPE_REPRESENTATION('',(#522),#12803);
#585=STYLED_ITEM('',(#13240),#616);
#586=STYLED_ITEM('',(#13240),#617);
#587=STYLED_ITEM('',(#13233),#618);
#588=STYLED_ITEM('',(#13261),#619);
#589=STYLED_ITEM('',(#13240),#620);
#590=STYLED_ITEM('',(#13240),#621);
#591=STYLED_ITEM('',(#13233),#622);
#592=STYLED_ITEM('',(#13261),#623);
#593=STYLED_ITEM('',(#13240),#624);
#594=STYLED_ITEM('',(#13240),#625);
#595=STYLED_ITEM('',(#13233),#626);
#596=STYLED_ITEM('',(#13261),#627);
#597=STYLED_ITEM('',(#13233),#628);
#598=STYLED_ITEM('',(#13261),#629);
#599=STYLED_ITEM('',(#13233),#630);
#600=STYLED_ITEM('',(#13240),#631);
#601=STYLED_ITEM('',(#13254),#518);
#602=STYLED_ITEM('',(#13254),#632);
#603=STYLED_ITEM('',(#13254),#519);
#604=STYLED_ITEM('',(#13233),#633);
#605=STYLED_ITEM('',(#13254),#634);
#606=STYLED_ITEM('',(#13226),#635);
#607=STYLED_ITEM('',(#13226),#636);
#608=STYLED_ITEM('',(#13240),#637);
#609=STYLED_ITEM('',(#13261),#638);
#610=STYLED_ITEM('',(#13254),#639);
#611=STYLED_ITEM('',(#13254),#520);
#612=STYLED_ITEM('',(#13254),#640);
#613=STYLED_ITEM('',(#13254),#521);
#614=STYLED_ITEM('',(#13254),#641);
#615=STYLED_ITEM('',(#13254),#522);
#616=MANIFOLD_SOLID_BREP('Body1',#7363);
#617=MANIFOLD_SOLID_BREP('Body1',#7364);
#618=MANIFOLD_SOLID_BREP('Body1',#7365);
#619=MANIFOLD_SOLID_BREP('Body1',#7366);
#620=MANIFOLD_SOLID_BREP('Body1',#7367);
#621=MANIFOLD_SOLID_BREP('Body1',#7368);
#622=MANIFOLD_SOLID_BREP('Body1',#7369);
#623=MANIFOLD_SOLID_BREP('Body1',#7370);
#624=MANIFOLD_SOLID_BREP('Body1',#7371);
#625=MANIFOLD_SOLID_BREP('Body1',#7372);
#626=MANIFOLD_SOLID_BREP('Body1',#7373);
#627=MANIFOLD_SOLID_BREP('Body1',#7374);
#628=MANIFOLD_SOLID_BREP('Body1',#7375);
#629=MANIFOLD_SOLID_BREP('Body1',#7376);
#630=MANIFOLD_SOLID_BREP('Body1',#7377);
#631=MANIFOLD_SOLID_BREP('Body1',#7378);
#632=MANIFOLD_SOLID_BREP('Body1',#7381);
#633=MANIFOLD_SOLID_BREP('Body1',#7384);
#634=MANIFOLD_SOLID_BREP('Body1',#7385);
#635=MANIFOLD_SOLID_BREP('Body1',#7386);
#636=MANIFOLD_SOLID_BREP('Body1',#7387);
#637=MANIFOLD_SOLID_BREP('Body1',#7388);
#638=MANIFOLD_SOLID_BREP('Body1',#7389);
#639=MANIFOLD_SOLID_BREP('Body1',#7390);
#640=MANIFOLD_SOLID_BREP('Body1',#7393);
#641=MANIFOLD_SOLID_BREP('Body1',#7396);
#642=FACE_BOUND('',#1448,.T.);
#643=FACE_BOUND('',#1449,.T.);
#644=FACE_BOUND('',#1450,.T.);
#645=FACE_BOUND('',#1451,.T.);
#646=FACE_BOUND('',#1452,.T.);
#647=FACE_BOUND('',#1453,.T.);
#648=FACE_BOUND('',#1455,.T.);
#649=FACE_BOUND('',#1456,.T.);
#650=FACE_BOUND('',#1457,.T.);
#651=FACE_BOUND('',#1458,.T.);
#652=FACE_BOUND('',#1459,.T.);
#653=FACE_BOUND('',#1460,.T.);
#654=FACE_BOUND('',#1472,.T.);
#655=FACE_BOUND('',#1473,.T.);
#656=FACE_BOUND('',#1474,.T.);
#657=FACE_BOUND('',#1475,.T.);
#658=FACE_BOUND('',#1476,.T.);
#659=FACE_BOUND('',#1477,.T.);
#660=FACE_BOUND('',#1479,.T.);
#661=FACE_BOUND('',#1480,.T.);
#662=FACE_BOUND('',#1481,.T.);
#663=FACE_BOUND('',#1482,.T.);
#664=FACE_BOUND('',#1483,.T.);
#665=FACE_BOUND('',#1484,.T.);
#666=FACE_BOUND('',#1492,.T.);
#667=FACE_BOUND('',#1493,.T.);
#668=FACE_BOUND('',#1495,.T.);
#669=FACE_BOUND('',#1496,.T.);
#670=FACE_BOUND('',#1504,.T.);
#671=FACE_BOUND('',#1505,.T.);
#672=FACE_BOUND('',#1507,.T.);
#673=FACE_BOUND('',#1508,.T.);
#674=FACE_BOUND('',#1528,.T.);
#675=FACE_BOUND('',#1529,.T.);
#676=FACE_BOUND('',#1531,.T.);
#677=FACE_BOUND('',#1532,.T.);
#678=FACE_BOUND('',#1540,.T.);
#679=FACE_BOUND('',#1541,.T.);
#680=FACE_BOUND('',#1543,.T.);
#681=FACE_BOUND('',#1544,.T.);
#682=FACE_BOUND('',#1560,.T.);
#683=FACE_BOUND('',#1564,.T.);
#684=FACE_BOUND('',#1575,.T.);
#685=FACE_BOUND('',#1576,.T.);
#686=FACE_BOUND('',#1586,.T.);
#687=FACE_BOUND('',#1590,.T.);
#688=FACE_BOUND('',#1601,.T.);
#689=FACE_BOUND('',#1602,.T.);
#690=FACE_BOUND('',#1655,.T.);
#691=FACE_BOUND('',#1657,.T.);
#692=FACE_BOUND('',#1660,.T.);
#693=FACE_BOUND('',#1663,.T.);
#694=FACE_BOUND('',#1666,.T.);
#695=FACE_BOUND('',#1669,.T.);
#696=FACE_BOUND('',#1679,.T.);
#697=FACE_BOUND('',#1680,.T.);
#698=FACE_BOUND('',#1681,.T.);
#699=FACE_BOUND('',#1682,.T.);
#700=FACE_BOUND('',#1689,.T.);
#701=FACE_BOUND('',#1690,.T.);
#702=FACE_BOUND('',#1691,.T.);
#703=FACE_BOUND('',#1692,.T.);
#704=FACE_BOUND('',#1701,.T.);
#705=FACE_BOUND('',#1717,.T.);
#706=FACE_BOUND('',#1743,.T.);
#707=FACE_BOUND('',#1770,.T.);
#708=FACE_BOUND('',#1771,.T.);
#709=FACE_BOUND('',#1772,.T.);
#710=FACE_BOUND('',#1773,.T.);
#711=FACE_BOUND('',#1774,.T.);
#712=FACE_BOUND('',#1775,.T.);
#713=FACE_BOUND('',#1776,.T.);
#714=FACE_BOUND('',#1777,.T.);
#715=FACE_BOUND('',#1778,.T.);
#716=FACE_BOUND('',#1779,.T.);
#717=FACE_BOUND('',#1780,.T.);
#718=FACE_BOUND('',#1781,.T.);
#719=FACE_BOUND('',#1782,.T.);
#720=FACE_BOUND('',#1783,.T.);
#721=FACE_BOUND('',#1784,.T.);
#722=FACE_BOUND('',#1785,.T.);
#723=FACE_BOUND('',#1786,.T.);
#724=FACE_BOUND('',#1787,.T.);
#725=FACE_BOUND('',#1788,.T.);
#726=FACE_BOUND('',#1790,.T.);
#727=FACE_BOUND('',#1791,.T.);
#728=FACE_BOUND('',#1792,.T.);
#729=FACE_BOUND('',#1793,.T.);
#730=FACE_BOUND('',#1794,.T.);
#731=FACE_BOUND('',#1795,.T.);
#732=FACE_BOUND('',#1796,.T.);
#733=FACE_BOUND('',#1797,.T.);
#734=FACE_BOUND('',#1798,.T.);
#735=FACE_BOUND('',#1799,.T.);
#736=FACE_BOUND('',#1800,.T.);
#737=FACE_BOUND('',#1801,.T.);
#738=FACE_BOUND('',#1802,.T.);
#739=FACE_BOUND('',#1803,.T.);
#740=FACE_BOUND('',#1804,.T.);
#741=FACE_BOUND('',#1805,.T.);
#742=FACE_BOUND('',#1806,.T.);
#743=FACE_BOUND('',#1807,.T.);
#744=FACE_BOUND('',#1808,.T.);
#745=FACE_BOUND('',#1812,.T.);
#746=FACE_BOUND('',#1814,.T.);
#747=FACE_BOUND('',#1818,.T.);
#748=FACE_BOUND('',#1819,.T.);
#749=FACE_BOUND('',#1824,.T.);
#750=FACE_BOUND('',#1825,.T.);
#751=FACE_BOUND('',#1843,.T.);
#752=FACE_BOUND('',#1844,.T.);
#753=FACE_BOUND('',#1845,.T.);
#754=FACE_BOUND('',#1846,.T.);
#755=FACE_BOUND('',#1878,.T.);
#756=FACE_BOUND('',#1881,.T.);
#757=FACE_BOUND('',#1887,.T.);
#758=FACE_BOUND('',#1903,.T.);
#759=FACE_BOUND('',#1905,.T.);
#760=FACE_BOUND('',#1911,.T.);
#761=FACE_BOUND('',#1927,.T.);
#762=FACE_BOUND('',#1930,.T.);
#763=FACE_BOUND('',#1945,.T.);
#764=PLANE('',#7762);
#765=PLANE('',#7763);
#766=PLANE('',#7764);
#767=PLANE('',#7765);
#768=PLANE('',#7766);
#769=PLANE('',#7767);
#770=PLANE('',#7787);
#771=PLANE('',#7788);
#772=PLANE('',#7789);
#773=PLANE('',#7790);
#774=PLANE('',#7791);
#775=PLANE('',#7792);
#776=PLANE('',#7800);
#777=PLANE('',#7801);
#778=PLANE('',#7802);
#779=PLANE('',#7803);
#780=PLANE('',#7804);
#781=PLANE('',#7805);
#782=PLANE('',#7813);
#783=PLANE('',#7814);
#784=PLANE('',#7815);
#785=PLANE('',#7816);
#786=PLANE('',#7817);
#787=PLANE('',#7818);
#788=PLANE('',#7820);
#789=PLANE('',#7821);
#790=PLANE('',#7822);
#791=PLANE('',#7823);
#792=PLANE('',#7824);
#793=PLANE('',#7825);
#794=PLANE('',#7827);
#795=PLANE('',#7828);
#796=PLANE('',#7829);
#797=PLANE('',#7830);
#798=PLANE('',#7831);
#799=PLANE('',#7832);
#800=PLANE('',#7840);
#801=PLANE('',#7841);
#802=PLANE('',#7842);
#803=PLANE('',#7843);
#804=PLANE('',#7844);
#805=PLANE('',#7845);
#806=PLANE('',#7853);
#807=PLANE('',#7854);
#808=PLANE('',#7855);
#809=PLANE('',#7856);
#810=PLANE('',#7857);
#811=PLANE('',#7858);
#812=PLANE('',#7860);
#813=PLANE('',#7861);
#814=PLANE('',#7862);
#815=PLANE('',#7863);
#816=PLANE('',#7864);
#817=PLANE('',#7865);
#818=PLANE('',#7867);
#819=PLANE('',#7868);
#820=PLANE('',#7869);
#821=PLANE('',#7870);
#822=PLANE('',#7871);
#823=PLANE('',#7872);
#824=PLANE('',#7880);
#825=PLANE('',#7888);
#826=PLANE('',#7890);
#827=PLANE('',#7891);
#828=PLANE('',#7892);
#829=PLANE('',#7897);
#830=PLANE('',#7898);
#831=PLANE('',#7899);
#832=PLANE('',#7900);
#833=PLANE('',#7901);
#834=PLANE('',#7903);
#835=PLANE('',#7904);
#836=PLANE('',#7905);
#837=PLANE('',#7906);
#838=PLANE('',#7907);
#839=PLANE('',#7908);
#840=PLANE('',#7916);
#841=PLANE('',#7924);
#842=PLANE('',#7926);
#843=PLANE('',#7927);
#844=PLANE('',#7928);
#845=PLANE('',#7933);
#846=PLANE('',#7934);
#847=PLANE('',#7935);
#848=PLANE('',#7936);
#849=PLANE('',#7937);
#850=PLANE('',#7939);
#851=PLANE('',#7940);
#852=PLANE('',#7941);
#853=PLANE('',#7942);
#854=PLANE('',#7943);
#855=PLANE('',#7944);
#856=PLANE('',#7946);
#857=PLANE('',#7947);
#858=PLANE('',#7948);
#859=PLANE('',#7949);
#860=PLANE('',#7950);
#861=PLANE('',#7951);
#862=PLANE('',#7952);
#863=PLANE('',#7953);
#864=PLANE('',#7954);
#865=PLANE('',#7955);
#866=PLANE('',#7956);
#867=PLANE('',#7957);
#868=PLANE('',#7958);
#869=PLANE('',#7959);
#870=PLANE('',#7960);
#871=PLANE('',#7961);
#872=PLANE('',#7962);
#873=PLANE('',#7963);
#874=PLANE('',#7964);
#875=PLANE('',#7965);
#876=PLANE('',#7966);
#877=PLANE('',#7967);
#878=PLANE('',#7968);
#879=PLANE('',#7969);
#880=PLANE('',#7970);
#881=PLANE('',#7971);
#882=PLANE('',#7972);
#883=PLANE('',#7973);
#884=PLANE('',#7974);
#885=PLANE('',#7975);
#886=PLANE('',#7976);
#887=PLANE('',#7977);
#888=PLANE('',#7978);
#889=PLANE('',#7979);
#890=PLANE('',#7980);
#891=PLANE('',#7981);
#892=PLANE('',#7985);
#893=PLANE('',#7986);
#894=PLANE('',#7987);
#895=PLANE('',#7988);
#896=PLANE('',#7989);
#897=PLANE('',#7990);
#898=PLANE('',#7991);
#899=PLANE('',#7992);
#900=PLANE('',#7993);
#901=PLANE('',#7994);
#902=PLANE('',#7999);
#903=PLANE('',#8004);
#904=PLANE('',#8009);
#905=PLANE('',#8014);
#906=PLANE('',#8024);
#907=PLANE('',#8025);
#908=PLANE('',#8026);
#909=PLANE('',#8027);
#910=PLANE('',#8028);
#911=PLANE('',#8029);
#912=PLANE('',#8030);
#913=PLANE('',#8031);
#914=PLANE('',#8032);
#915=PLANE('',#8033);
#916=PLANE('',#8034);
#917=PLANE('',#8035);
#918=PLANE('',#8036);
#919=PLANE('',#8037);
#920=PLANE('',#8039);
#921=PLANE('',#8047);
#922=PLANE('',#8055);
#923=PLANE('',#8056);
#924=PLANE('',#8057);
#925=PLANE('',#8058);
#926=PLANE('',#8059);
#927=PLANE('',#8060);
#928=PLANE('',#8061);
#929=PLANE('',#8062);
#930=PLANE('',#8063);
#931=PLANE('',#8065);
#932=PLANE('',#8066);
#933=PLANE('',#8067);
#934=PLANE('',#8069);
#935=PLANE('',#8070);
#936=PLANE('',#8071);
#937=PLANE('',#8072);
#938=PLANE('',#8073);
#939=PLANE('',#8074);
#940=PLANE('',#8081);
#941=PLANE('',#8082);
#942=PLANE('',#8083);
#943=PLANE('',#8084);
#944=PLANE('',#8086);
#945=PLANE('',#8087);
#946=PLANE('',#8088);
#947=PLANE('',#8089);
#948=PLANE('',#8090);
#949=PLANE('',#8091);
#950=PLANE('',#8092);
#951=PLANE('',#8093);
#952=PLANE('',#8094);
#953=PLANE('',#8096);
#954=PLANE('',#8104);
#955=PLANE('',#8168);
#956=PLANE('',#8169);
#957=PLANE('',#8170);
#958=PLANE('',#8171);
#959=PLANE('',#8172);
#960=PLANE('',#8173);
#961=PLANE('',#8181);
#962=PLANE('',#8182);
#963=PLANE('',#8190);
#964=PLANE('',#8191);
#965=PLANE('',#8192);
#966=PLANE('',#8193);
#967=PLANE('',#8194);
#968=PLANE('',#8195);
#969=PLANE('',#8196);
#970=PLANE('',#8197);
#971=PLANE('',#8200);
#972=PLANE('',#8206);
#973=PLANE('',#8212);
#974=PLANE('',#8218);
#975=PLANE('',#8224);
#976=PLANE('',#8225);
#977=PLANE('',#8226);
#978=PLANE('',#8227);
#979=PLANE('',#8228);
#980=PLANE('',#8229);
#981=PLANE('',#8230);
#982=PLANE('',#8231);
#983=PLANE('',#8232);
#984=PLANE('',#8233);
#985=PLANE('',#8234);
#986=PLANE('',#8235);
#987=PLANE('',#8236);
#988=PLANE('',#8237);
#989=PLANE('',#8239);
#990=PLANE('',#8240);
#991=PLANE('',#8241);
#992=PLANE('',#8242);
#993=PLANE('',#8243);
#994=PLANE('',#8244);
#995=PLANE('',#8245);
#996=PLANE('',#8246);
#997=PLANE('',#8247);
#998=PLANE('',#8248);
#999=PLANE('',#8250);
#1000=PLANE('',#8251);
#1001=PLANE('',#8252);
#1002=PLANE('',#8253);
#1003=PLANE('',#8254);
#1004=PLANE('',#8255);
#1005=PLANE('',#8256);
#1006=PLANE('',#8257);
#1007=PLANE('',#8258);
#1008=PLANE('',#8259);
#1009=PLANE('',#8269);
#1010=PLANE('',#8273);
#1011=PLANE('',#8345);
#1012=PLANE('',#8353);
#1013=PLANE('',#8361);
#1014=PLANE('',#8362);
#1015=PLANE('',#8363);
#1016=PLANE('',#8364);
#1017=PLANE('',#8365);
#1018=PLANE('',#8366);
#1019=PLANE('',#8367);
#1020=PLANE('',#8368);
#1021=PLANE('',#8369);
#1022=PLANE('',#8377);
#1023=PLANE('',#8378);
#1024=PLANE('',#8380);
#1025=PLANE('',#8388);
#1026=PLANE('',#8396);
#1027=PLANE('',#8397);
#1028=PLANE('',#8398);
#1029=PLANE('',#8399);
#1030=PLANE('',#8400);
#1031=PLANE('',#8401);
#1032=PLANE('',#8402);
#1033=PLANE('',#8403);
#1034=PLANE('',#8404);
#1035=PLANE('',#8411);
#1036=PLANE('',#8415);
#1037=PLANE('',#8417);
#1038=PLANE('',#8418);
#1039=PLANE('',#8419);
#1040=PLANE('',#8420);
#1041=PLANE('',#8421);
#1042=PLANE('',#8422);
#1043=PLANE('',#8423);
#1044=PLANE('',#8424);
#1045=PLANE('',#8425);
#1046=PLANE('',#8427);
#1047=PLANE('',#8435);
#1048=FACE_OUTER_BOUND('',#1437,.T.);
#1049=FACE_OUTER_BOUND('',#1438,.T.);
#1050=FACE_OUTER_BOUND('',#1439,.T.);
#1051=FACE_OUTER_BOUND('',#1440,.T.);
#1052=FACE_OUTER_BOUND('',#1441,.T.);
#1053=FACE_OUTER_BOUND('',#1442,.T.);
#1054=FACE_OUTER_BOUND('',#1443,.T.);
#1055=FACE_OUTER_BOUND('',#1444,.T.);
#1056=FACE_OUTER_BOUND('',#1445,.T.);
#1057=FACE_OUTER_BOUND('',#1446,.T.);
#1058=FACE_OUTER_BOUND('',#1447,.T.);
#1059=FACE_OUTER_BOUND('',#1454,.T.);
#1060=FACE_OUTER_BOUND('',#1461,.T.);
#1061=FACE_OUTER_BOUND('',#1462,.T.);
#1062=FACE_OUTER_BOUND('',#1463,.T.);
#1063=FACE_OUTER_BOUND('',#1464,.T.);
#1064=FACE_OUTER_BOUND('',#1465,.T.);
#1065=FACE_OUTER_BOUND('',#1466,.T.);
#1066=FACE_OUTER_BOUND('',#1467,.T.);
#1067=FACE_OUTER_BOUND('',#1468,.T.);
#1068=FACE_OUTER_BOUND('',#1469,.T.);
#1069=FACE_OUTER_BOUND('',#1470,.T.);
#1070=FACE_OUTER_BOUND('',#1471,.T.);
#1071=FACE_OUTER_BOUND('',#1478,.T.);
#1072=FACE_OUTER_BOUND('',#1485,.T.);
#1073=FACE_OUTER_BOUND('',#1486,.T.);
#1074=FACE_OUTER_BOUND('',#1487,.T.);
#1075=FACE_OUTER_BOUND('',#1488,.T.);
#1076=FACE_OUTER_BOUND('',#1489,.T.);
#1077=FACE_OUTER_BOUND('',#1490,.T.);
#1078=FACE_OUTER_BOUND('',#1491,.T.);
#1079=FACE_OUTER_BOUND('',#1494,.T.);
#1080=FACE_OUTER_BOUND('',#1497,.T.);
#1081=FACE_OUTER_BOUND('',#1498,.T.);
#1082=FACE_OUTER_BOUND('',#1499,.T.);
#1083=FACE_OUTER_BOUND('',#1500,.T.);
#1084=FACE_OUTER_BOUND('',#1501,.T.);
#1085=FACE_OUTER_BOUND('',#1502,.T.);
#1086=FACE_OUTER_BOUND('',#1503,.T.);
#1087=FACE_OUTER_BOUND('',#1506,.T.);
#1088=FACE_OUTER_BOUND('',#1509,.T.);
#1089=FACE_OUTER_BOUND('',#1510,.T.);
#1090=FACE_OUTER_BOUND('',#1511,.T.);
#1091=FACE_OUTER_BOUND('',#1512,.T.);
#1092=FACE_OUTER_BOUND('',#1513,.T.);
#1093=FACE_OUTER_BOUND('',#1514,.T.);
#1094=FACE_OUTER_BOUND('',#1515,.T.);
#1095=FACE_OUTER_BOUND('',#1516,.T.);
#1096=FACE_OUTER_BOUND('',#1517,.T.);
#1097=FACE_OUTER_BOUND('',#1518,.T.);
#1098=FACE_OUTER_BOUND('',#1519,.T.);
#1099=FACE_OUTER_BOUND('',#1520,.T.);
#1100=FACE_OUTER_BOUND('',#1521,.T.);
#1101=FACE_OUTER_BOUND('',#1522,.T.);
#1102=FACE_OUTER_BOUND('',#1523,.T.);
#1103=FACE_OUTER_BOUND('',#1524,.T.);
#1104=FACE_OUTER_BOUND('',#1525,.T.);
#1105=FACE_OUTER_BOUND('',#1526,.T.);
#1106=FACE_OUTER_BOUND('',#1527,.T.);
#1107=FACE_OUTER_BOUND('',#1530,.T.);
#1108=FACE_OUTER_BOUND('',#1533,.T.);
#1109=FACE_OUTER_BOUND('',#1534,.T.);
#1110=FACE_OUTER_BOUND('',#1535,.T.);
#1111=FACE_OUTER_BOUND('',#1536,.T.);
#1112=FACE_OUTER_BOUND('',#1537,.T.);
#1113=FACE_OUTER_BOUND('',#1538,.T.);
#1114=FACE_OUTER_BOUND('',#1539,.T.);
#1115=FACE_OUTER_BOUND('',#1542,.T.);
#1116=FACE_OUTER_BOUND('',#1545,.T.);
#1117=FACE_OUTER_BOUND('',#1546,.T.);
#1118=FACE_OUTER_BOUND('',#1547,.T.);
#1119=FACE_OUTER_BOUND('',#1548,.T.);
#1120=FACE_OUTER_BOUND('',#1549,.T.);
#1121=FACE_OUTER_BOUND('',#1550,.T.);
#1122=FACE_OUTER_BOUND('',#1551,.T.);
#1123=FACE_OUTER_BOUND('',#1552,.T.);
#1124=FACE_OUTER_BOUND('',#1553,.T.);
#1125=FACE_OUTER_BOUND('',#1554,.T.);
#1126=FACE_OUTER_BOUND('',#1555,.T.);
#1127=FACE_OUTER_BOUND('',#1556,.T.);
#1128=FACE_OUTER_BOUND('',#1557,.T.);
#1129=FACE_OUTER_BOUND('',#1558,.T.);
#1130=FACE_OUTER_BOUND('',#1559,.T.);
#1131=FACE_OUTER_BOUND('',#1561,.T.);
#1132=FACE_OUTER_BOUND('',#1562,.T.);
#1133=FACE_OUTER_BOUND('',#1563,.T.);
#1134=FACE_OUTER_BOUND('',#1565,.T.);
#1135=FACE_OUTER_BOUND('',#1566,.T.);
#1136=FACE_OUTER_BOUND('',#1567,.T.);
#1137=FACE_OUTER_BOUND('',#1568,.T.);
#1138=FACE_OUTER_BOUND('',#1569,.T.);
#1139=FACE_OUTER_BOUND('',#1570,.T.);
#1140=FACE_OUTER_BOUND('',#1571,.T.);
#1141=FACE_OUTER_BOUND('',#1572,.T.);
#1142=FACE_OUTER_BOUND('',#1573,.T.);
#1143=FACE_OUTER_BOUND('',#1574,.T.);
#1144=FACE_OUTER_BOUND('',#1577,.T.);
#1145=FACE_OUTER_BOUND('',#1578,.T.);
#1146=FACE_OUTER_BOUND('',#1579,.T.);
#1147=FACE_OUTER_BOUND('',#1580,.T.);
#1148=FACE_OUTER_BOUND('',#1581,.T.);
#1149=FACE_OUTER_BOUND('',#1582,.T.);
#1150=FACE_OUTER_BOUND('',#1583,.T.);
#1151=FACE_OUTER_BOUND('',#1584,.T.);
#1152=FACE_OUTER_BOUND('',#1585,.T.);
#1153=FACE_OUTER_BOUND('',#1587,.T.);
#1154=FACE_OUTER_BOUND('',#1588,.T.);
#1155=FACE_OUTER_BOUND('',#1589,.T.);
#1156=FACE_OUTER_BOUND('',#1591,.T.);
#1157=FACE_OUTER_BOUND('',#1592,.T.);
#1158=FACE_OUTER_BOUND('',#1593,.T.);
#1159=FACE_OUTER_BOUND('',#1594,.T.);
#1160=FACE_OUTER_BOUND('',#1595,.T.);
#1161=FACE_OUTER_BOUND('',#1596,.T.);
#1162=FACE_OUTER_BOUND('',#1597,.T.);
#1163=FACE_OUTER_BOUND('',#1598,.T.);
#1164=FACE_OUTER_BOUND('',#1599,.T.);
#1165=FACE_OUTER_BOUND('',#1600,.T.);
#1166=FACE_OUTER_BOUND('',#1603,.T.);
#1167=FACE_OUTER_BOUND('',#1604,.T.);
#1168=FACE_OUTER_BOUND('',#1605,.T.);
#1169=FACE_OUTER_BOUND('',#1606,.T.);
#1170=FACE_OUTER_BOUND('',#1607,.T.);
#1171=FACE_OUTER_BOUND('',#1608,.T.);
#1172=FACE_OUTER_BOUND('',#1609,.T.);
#1173=FACE_OUTER_BOUND('',#1610,.T.);
#1174=FACE_OUTER_BOUND('',#1611,.T.);
#1175=FACE_OUTER_BOUND('',#1612,.T.);
#1176=FACE_OUTER_BOUND('',#1613,.T.);
#1177=FACE_OUTER_BOUND('',#1614,.T.);
#1178=FACE_OUTER_BOUND('',#1615,.T.);
#1179=FACE_OUTER_BOUND('',#1616,.T.);
#1180=FACE_OUTER_BOUND('',#1617,.T.);
#1181=FACE_OUTER_BOUND('',#1618,.T.);
#1182=FACE_OUTER_BOUND('',#1619,.T.);
#1183=FACE_OUTER_BOUND('',#1620,.T.);
#1184=FACE_OUTER_BOUND('',#1621,.T.);
#1185=FACE_OUTER_BOUND('',#1622,.T.);
#1186=FACE_OUTER_BOUND('',#1623,.T.);
#1187=FACE_OUTER_BOUND('',#1624,.T.);
#1188=FACE_OUTER_BOUND('',#1625,.T.);
#1189=FACE_OUTER_BOUND('',#1626,.T.);
#1190=FACE_OUTER_BOUND('',#1627,.T.);
#1191=FACE_OUTER_BOUND('',#1628,.T.);
#1192=FACE_OUTER_BOUND('',#1629,.T.);
#1193=FACE_OUTER_BOUND('',#1630,.T.);
#1194=FACE_OUTER_BOUND('',#1631,.T.);
#1195=FACE_OUTER_BOUND('',#1632,.T.);
#1196=FACE_OUTER_BOUND('',#1633,.T.);
#1197=FACE_OUTER_BOUND('',#1634,.T.);
#1198=FACE_OUTER_BOUND('',#1635,.T.);
#1199=FACE_OUTER_BOUND('',#1636,.T.);
#1200=FACE_OUTER_BOUND('',#1637,.T.);
#1201=FACE_OUTER_BOUND('',#1638,.T.);
#1202=FACE_OUTER_BOUND('',#1639,.T.);
#1203=FACE_OUTER_BOUND('',#1640,.T.);
#1204=FACE_OUTER_BOUND('',#1641,.T.);
#1205=FACE_OUTER_BOUND('',#1642,.T.);
#1206=FACE_OUTER_BOUND('',#1643,.T.);
#1207=FACE_OUTER_BOUND('',#1644,.T.);
#1208=FACE_OUTER_BOUND('',#1645,.T.);
#1209=FACE_OUTER_BOUND('',#1646,.T.);
#1210=FACE_OUTER_BOUND('',#1647,.T.);
#1211=FACE_OUTER_BOUND('',#1648,.T.);
#1212=FACE_OUTER_BOUND('',#1649,.T.);
#1213=FACE_OUTER_BOUND('',#1650,.T.);
#1214=FACE_OUTER_BOUND('',#1651,.T.);
#1215=FACE_OUTER_BOUND('',#1652,.T.);
#1216=FACE_OUTER_BOUND('',#1653,.T.);
#1217=FACE_OUTER_BOUND('',#1654,.T.);
#1218=FACE_OUTER_BOUND('',#1656,.T.);
#1219=FACE_OUTER_BOUND('',#1658,.T.);
#1220=FACE_OUTER_BOUND('',#1659,.T.);
#1221=FACE_OUTER_BOUND('',#1661,.T.);
#1222=FACE_OUTER_BOUND('',#1662,.T.);
#1223=FACE_OUTER_BOUND('',#1664,.T.);
#1224=FACE_OUTER_BOUND('',#1665,.T.);
#1225=FACE_OUTER_BOUND('',#1667,.T.);
#1226=FACE_OUTER_BOUND('',#1668,.T.);
#1227=FACE_OUTER_BOUND('',#1670,.T.);
#1228=FACE_OUTER_BOUND('',#1671,.T.);
#1229=FACE_OUTER_BOUND('',#1672,.T.);
#1230=FACE_OUTER_BOUND('',#1673,.T.);
#1231=FACE_OUTER_BOUND('',#1674,.T.);
#1232=FACE_OUTER_BOUND('',#1675,.T.);
#1233=FACE_OUTER_BOUND('',#1676,.T.);
#1234=FACE_OUTER_BOUND('',#1677,.T.);
#1235=FACE_OUTER_BOUND('',#1678,.T.);
#1236=FACE_OUTER_BOUND('',#1683,.T.);
#1237=FACE_OUTER_BOUND('',#1684,.T.);
#1238=FACE_OUTER_BOUND('',#1685,.T.);
#1239=FACE_OUTER_BOUND('',#1686,.T.);
#1240=FACE_OUTER_BOUND('',#1687,.T.);
#1241=FACE_OUTER_BOUND('',#1688,.T.);
#1242=FACE_OUTER_BOUND('',#1693,.T.);
#1243=FACE_OUTER_BOUND('',#1694,.T.);
#1244=FACE_OUTER_BOUND('',#1695,.T.);
#1245=FACE_OUTER_BOUND('',#1696,.T.);
#1246=FACE_OUTER_BOUND('',#1697,.T.);
#1247=FACE_OUTER_BOUND('',#1698,.T.);
#1248=FACE_OUTER_BOUND('',#1699,.T.);
#1249=FACE_OUTER_BOUND('',#1700,.T.);
#1250=FACE_OUTER_BOUND('',#1702,.T.);
#1251=FACE_OUTER_BOUND('',#1703,.T.);
#1252=FACE_OUTER_BOUND('',#1704,.T.);
#1253=FACE_OUTER_BOUND('',#1705,.T.);
#1254=FACE_OUTER_BOUND('',#1706,.T.);
#1255=FACE_OUTER_BOUND('',#1707,.T.);
#1256=FACE_OUTER_BOUND('',#1708,.T.);
#1257=FACE_OUTER_BOUND('',#1709,.T.);
#1258=FACE_OUTER_BOUND('',#1710,.T.);
#1259=FACE_OUTER_BOUND('',#1711,.T.);
#1260=FACE_OUTER_BOUND('',#1712,.T.);
#1261=FACE_OUTER_BOUND('',#1713,.T.);
#1262=FACE_OUTER_BOUND('',#1714,.T.);
#1263=FACE_OUTER_BOUND('',#1715,.T.);
#1264=FACE_OUTER_BOUND('',#1716,.T.);
#1265=FACE_OUTER_BOUND('',#1718,.T.);
#1266=FACE_OUTER_BOUND('',#1719,.T.);
#1267=FACE_OUTER_BOUND('',#1720,.T.);
#1268=FACE_OUTER_BOUND('',#1721,.T.);
#1269=FACE_OUTER_BOUND('',#1722,.T.);
#1270=FACE_OUTER_BOUND('',#1723,.T.);
#1271=FACE_OUTER_BOUND('',#1724,.T.);
#1272=FACE_OUTER_BOUND('',#1725,.T.);
#1273=FACE_OUTER_BOUND('',#1726,.T.);
#1274=FACE_OUTER_BOUND('',#1727,.T.);
#1275=FACE_OUTER_BOUND('',#1728,.T.);
#1276=FACE_OUTER_BOUND('',#1729,.T.);
#1277=FACE_OUTER_BOUND('',#1730,.T.);
#1278=FACE_OUTER_BOUND('',#1731,.T.);
#1279=FACE_OUTER_BOUND('',#1732,.T.);
#1280=FACE_OUTER_BOUND('',#1733,.T.);
#1281=FACE_OUTER_BOUND('',#1734,.T.);
#1282=FACE_OUTER_BOUND('',#1735,.T.);
#1283=FACE_OUTER_BOUND('',#1736,.T.);
#1284=FACE_OUTER_BOUND('',#1737,.T.);
#1285=FACE_OUTER_BOUND('',#1738,.T.);
#1286=FACE_OUTER_BOUND('',#1739,.T.);
#1287=FACE_OUTER_BOUND('',#1740,.T.);
#1288=FACE_OUTER_BOUND('',#1741,.T.);
#1289=FACE_OUTER_BOUND('',#1742,.T.);
#1290=FACE_OUTER_BOUND('',#1744,.T.);
#1291=FACE_OUTER_BOUND('',#1745,.T.);
#1292=FACE_OUTER_BOUND('',#1746,.T.);
#1293=FACE_OUTER_BOUND('',#1747,.T.);
#1294=FACE_OUTER_BOUND('',#1748,.T.);
#1295=FACE_OUTER_BOUND('',#1749,.T.);
#1296=FACE_OUTER_BOUND('',#1750,.T.);
#1297=FACE_OUTER_BOUND('',#1751,.T.);
#1298=FACE_OUTER_BOUND('',#1752,.T.);
#1299=FACE_OUTER_BOUND('',#1753,.T.);
#1300=FACE_OUTER_BOUND('',#1754,.T.);
#1301=FACE_OUTER_BOUND('',#1755,.T.);
#1302=FACE_OUTER_BOUND('',#1756,.T.);
#1303=FACE_OUTER_BOUND('',#1757,.T.);
#1304=FACE_OUTER_BOUND('',#1758,.T.);
#1305=FACE_OUTER_BOUND('',#1759,.T.);
#1306=FACE_OUTER_BOUND('',#1760,.T.);
#1307=FACE_OUTER_BOUND('',#1761,.T.);
#1308=FACE_OUTER_BOUND('',#1762,.T.);
#1309=FACE_OUTER_BOUND('',#1763,.T.);
#1310=FACE_OUTER_BOUND('',#1764,.T.);
#1311=FACE_OUTER_BOUND('',#1765,.T.);
#1312=FACE_OUTER_BOUND('',#1766,.T.);
#1313=FACE_OUTER_BOUND('',#1767,.T.);
#1314=FACE_OUTER_BOUND('',#1768,.T.);
#1315=FACE_OUTER_BOUND('',#1769,.T.);
#1316=FACE_OUTER_BOUND('',#1789,.T.);
#1317=FACE_OUTER_BOUND('',#1809,.T.);
#1318=FACE_OUTER_BOUND('',#1810,.T.);
#1319=FACE_OUTER_BOUND('',#1811,.T.);
#1320=FACE_OUTER_BOUND('',#1813,.T.);
#1321=FACE_OUTER_BOUND('',#1815,.T.);
#1322=FACE_OUTER_BOUND('',#1816,.T.);
#1323=FACE_OUTER_BOUND('',#1817,.T.);
#1324=FACE_OUTER_BOUND('',#1820,.T.);
#1325=FACE_OUTER_BOUND('',#1821,.T.);
#1326=FACE_OUTER_BOUND('',#1822,.T.);
#1327=FACE_OUTER_BOUND('',#1823,.T.);
#1328=FACE_OUTER_BOUND('',#1826,.T.);
#1329=FACE_OUTER_BOUND('',#1827,.T.);
#1330=FACE_OUTER_BOUND('',#1828,.T.);
#1331=FACE_OUTER_BOUND('',#1829,.T.);
#1332=FACE_OUTER_BOUND('',#1830,.T.);
#1333=FACE_OUTER_BOUND('',#1831,.T.);
#1334=FACE_OUTER_BOUND('',#1832,.T.);
#1335=FACE_OUTER_BOUND('',#1833,.T.);
#1336=FACE_OUTER_BOUND('',#1834,.T.);
#1337=FACE_OUTER_BOUND('',#1835,.T.);
#1338=FACE_OUTER_BOUND('',#1836,.T.);
#1339=FACE_OUTER_BOUND('',#1837,.T.);
#1340=FACE_OUTER_BOUND('',#1838,.T.);
#1341=FACE_OUTER_BOUND('',#1839,.T.);
#1342=FACE_OUTER_BOUND('',#1840,.T.);
#1343=FACE_OUTER_BOUND('',#1841,.T.);
#1344=FACE_OUTER_BOUND('',#1842,.T.);
#1345=FACE_OUTER_BOUND('',#1847,.T.);
#1346=FACE_OUTER_BOUND('',#1848,.T.);
#1347=FACE_OUTER_BOUND('',#1849,.T.);
#1348=FACE_OUTER_BOUND('',#1850,.T.);
#1349=FACE_OUTER_BOUND('',#1851,.T.);
#1350=FACE_OUTER_BOUND('',#1852,.T.);
#1351=FACE_OUTER_BOUND('',#1853,.T.);
#1352=FACE_OUTER_BOUND('',#1854,.T.);
#1353=FACE_OUTER_BOUND('',#1855,.T.);
#1354=FACE_OUTER_BOUND('',#1856,.T.);
#1355=FACE_OUTER_BOUND('',#1857,.T.);
#1356=FACE_OUTER_BOUND('',#1858,.T.);
#1357=FACE_OUTER_BOUND('',#1859,.T.);
#1358=FACE_OUTER_BOUND('',#1860,.T.);
#1359=FACE_OUTER_BOUND('',#1861,.T.);
#1360=FACE_OUTER_BOUND('',#1862,.T.);
#1361=FACE_OUTER_BOUND('',#1863,.T.);
#1362=FACE_OUTER_BOUND('',#1864,.T.);
#1363=FACE_OUTER_BOUND('',#1865,.T.);
#1364=FACE_OUTER_BOUND('',#1866,.T.);
#1365=FACE_OUTER_BOUND('',#1867,.T.);
#1366=FACE_OUTER_BOUND('',#1868,.T.);
#1367=FACE_OUTER_BOUND('',#1869,.T.);
#1368=FACE_OUTER_BOUND('',#1870,.T.);
#1369=FACE_OUTER_BOUND('',#1871,.T.);
#1370=FACE_OUTER_BOUND('',#1872,.T.);
#1371=FACE_OUTER_BOUND('',#1873,.T.);
#1372=FACE_OUTER_BOUND('',#1874,.T.);
#1373=FACE_OUTER_BOUND('',#1875,.T.);
#1374=FACE_OUTER_BOUND('',#1876,.T.);
#1375=FACE_OUTER_BOUND('',#1877,.T.);
#1376=FACE_OUTER_BOUND('',#1879,.T.);
#1377=FACE_OUTER_BOUND('',#1880,.T.);
#1378=FACE_OUTER_BOUND('',#1882,.T.);
#1379=FACE_OUTER_BOUND('',#1883,.T.);
#1380=FACE_OUTER_BOUND('',#1884,.T.);
#1381=FACE_OUTER_BOUND('',#1885,.T.);
#1382=FACE_OUTER_BOUND('',#1886,.T.);
#1383=FACE_OUTER_BOUND('',#1888,.T.);
#1384=FACE_OUTER_BOUND('',#1889,.T.);
#1385=FACE_OUTER_BOUND('',#1890,.T.);
#1386=FACE_OUTER_BOUND('',#1891,.T.);
#1387=FACE_OUTER_BOUND('',#1892,.T.);
#1388=FACE_OUTER_BOUND('',#1893,.T.);
#1389=FACE_OUTER_BOUND('',#1894,.T.);
#1390=FACE_OUTER_BOUND('',#1895,.T.);
#1391=FACE_OUTER_BOUND('',#1896,.T.);
#1392=FACE_OUTER_BOUND('',#1897,.T.);
#1393=FACE_OUTER_BOUND('',#1898,.T.);
#1394=FACE_OUTER_BOUND('',#1899,.T.);
#1395=FACE_OUTER_BOUND('',#1900,.T.);
#1396=FACE_OUTER_BOUND('',#1901,.T.);
#1397=FACE_OUTER_BOUND('',#1902,.T.);
#1398=FACE_OUTER_BOUND('',#1904,.T.);
#1399=FACE_OUTER_BOUND('',#1906,.T.);
#1400=FACE_OUTER_BOUND('',#1907,.T.);
#1401=FACE_OUTER_BOUND('',#1908,.T.);
#1402=FACE_OUTER_BOUND('',#1909,.T.);
#1403=FACE_OUTER_BOUND('',#1910,.T.);
#1404=FACE_OUTER_BOUND('',#1912,.T.);
#1405=FACE_OUTER_BOUND('',#1913,.T.);
#1406=FACE_OUTER_BOUND('',#1914,.T.);
#1407=FACE_OUTER_BOUND('',#1915,.T.);
#1408=FACE_OUTER_BOUND('',#1916,.T.);
#1409=FACE_OUTER_BOUND('',#1917,.T.);
#1410=FACE_OUTER_BOUND('',#1918,.T.);
#1411=FACE_OUTER_BOUND('',#1919,.T.);
#1412=FACE_OUTER_BOUND('',#1920,.T.);
#1413=FACE_OUTER_BOUND('',#1921,.T.);
#1414=FACE_OUTER_BOUND('',#1922,.T.);
#1415=FACE_OUTER_BOUND('',#1923,.T.);
#1416=FACE_OUTER_BOUND('',#1924,.T.);
#1417=FACE_OUTER_BOUND('',#1925,.T.);
#1418=FACE_OUTER_BOUND('',#1926,.T.);
#1419=FACE_OUTER_BOUND('',#1928,.T.);
#1420=FACE_OUTER_BOUND('',#1929,.T.);
#1421=FACE_OUTER_BOUND('',#1931,.T.);
#1422=FACE_OUTER_BOUND('',#1932,.T.);
#1423=FACE_OUTER_BOUND('',#1933,.T.);
#1424=FACE_OUTER_BOUND('',#1934,.T.);
#1425=FACE_OUTER_BOUND('',#1935,.T.);
#1426=FACE_OUTER_BOUND('',#1936,.T.);
#1427=FACE_OUTER_BOUND('',#1937,.T.);
#1428=FACE_OUTER_BOUND('',#1938,.T.);
#1429=FACE_OUTER_BOUND('',#1939,.T.);
#1430=FACE_OUTER_BOUND('',#1940,.T.);
#1431=FACE_OUTER_BOUND('',#1941,.T.);
#1432=FACE_OUTER_BOUND('',#1942,.T.);
#1433=FACE_OUTER_BOUND('',#1943,.T.);
#1434=FACE_OUTER_BOUND('',#1944,.T.);
#1435=FACE_OUTER_BOUND('',#1946,.T.);
#1436=FACE_OUTER_BOUND('',#1947,.T.);
#1437=EDGE_LOOP('',(#5067,#5068,#5069,#5070));
#1438=EDGE_LOOP('',(#5071,#5072,#5073,#5074));
#1439=EDGE_LOOP('',(#5075,#5076,#5077,#5078));
#1440=EDGE_LOOP('',(#5079,#5080,#5081,#5082));
#1441=EDGE_LOOP('',(#5083,#5084,#5085,#5086));
#1442=EDGE_LOOP('',(#5087,#5088,#5089,#5090));
#1443=EDGE_LOOP('',(#5091,#5092,#5093,#5094));
#1444=EDGE_LOOP('',(#5095,#5096,#5097,#5098));
#1445=EDGE_LOOP('',(#5099,#5100,#5101,#5102));
#1446=EDGE_LOOP('',(#5103,#5104,#5105,#5106));
#1447=EDGE_LOOP('',(#5107,#5108,#5109,#5110));
#1448=EDGE_LOOP('',(#5111));
#1449=EDGE_LOOP('',(#5112));
#1450=EDGE_LOOP('',(#5113));
#1451=EDGE_LOOP('',(#5114));
#1452=EDGE_LOOP('',(#5115));
#1453=EDGE_LOOP('',(#5116));
#1454=EDGE_LOOP('',(#5117,#5118,#5119,#5120));
#1455=EDGE_LOOP('',(#5121));
#1456=EDGE_LOOP('',(#5122));
#1457=EDGE_LOOP('',(#5123));
#1458=EDGE_LOOP('',(#5124));
#1459=EDGE_LOOP('',(#5125));
#1460=EDGE_LOOP('',(#5126));
#1461=EDGE_LOOP('',(#5127,#5128,#5129,#5130));
#1462=EDGE_LOOP('',(#5131,#5132,#5133,#5134));
#1463=EDGE_LOOP('',(#5135,#5136,#5137,#5138));
#1464=EDGE_LOOP('',(#5139,#5140,#5141,#5142));
#1465=EDGE_LOOP('',(#5143,#5144,#5145,#5146));
#1466=EDGE_LOOP('',(#5147,#5148,#5149,#5150));
#1467=EDGE_LOOP('',(#5151,#5152,#5153,#5154));
#1468=EDGE_LOOP('',(#5155,#5156,#5157,#5158));
#1469=EDGE_LOOP('',(#5159,#5160,#5161,#5162));
#1470=EDGE_LOOP('',(#5163,#5164,#5165,#5166));
#1471=EDGE_LOOP('',(#5167,#5168,#5169,#5170));
#1472=EDGE_LOOP('',(#5171));
#1473=EDGE_LOOP('',(#5172));
#1474=EDGE_LOOP('',(#5173));
#1475=EDGE_LOOP('',(#5174));
#1476=EDGE_LOOP('',(#5175));
#1477=EDGE_LOOP('',(#5176));
#1478=EDGE_LOOP('',(#5177,#5178,#5179,#5180));
#1479=EDGE_LOOP('',(#5181));
#1480=EDGE_LOOP('',(#5182));
#1481=EDGE_LOOP('',(#5183));
#1482=EDGE_LOOP('',(#5184));
#1483=EDGE_LOOP('',(#5185));
#1484=EDGE_LOOP('',(#5186));
#1485=EDGE_LOOP('',(#5187,#5188,#5189,#5190));
#1486=EDGE_LOOP('',(#5191,#5192,#5193,#5194));
#1487=EDGE_LOOP('',(#5195,#5196,#5197,#5198));
#1488=EDGE_LOOP('',(#5199,#5200,#5201,#5202));
#1489=EDGE_LOOP('',(#5203,#5204,#5205,#5206));
#1490=EDGE_LOOP('',(#5207,#5208,#5209,#5210));
#1491=EDGE_LOOP('',(#5211,#5212,#5213,#5214));
#1492=EDGE_LOOP('',(#5215));
#1493=EDGE_LOOP('',(#5216));
#1494=EDGE_LOOP('',(#5217,#5218,#5219,#5220));
#1495=EDGE_LOOP('',(#5221));
#1496=EDGE_LOOP('',(#5222));
#1497=EDGE_LOOP('',(#5223,#5224,#5225,#5226));
#1498=EDGE_LOOP('',(#5227,#5228,#5229,#5230));
#1499=EDGE_LOOP('',(#5231,#5232,#5233,#5234));
#1500=EDGE_LOOP('',(#5235,#5236,#5237,#5238));
#1501=EDGE_LOOP('',(#5239,#5240,#5241,#5242));
#1502=EDGE_LOOP('',(#5243,#5244,#5245,#5246));
#1503=EDGE_LOOP('',(#5247,#5248,#5249,#5250));
#1504=EDGE_LOOP('',(#5251));
#1505=EDGE_LOOP('',(#5252));
#1506=EDGE_LOOP('',(#5253,#5254,#5255,#5256));
#1507=EDGE_LOOP('',(#5257));
#1508=EDGE_LOOP('',(#5258));
#1509=EDGE_LOOP('',(#5259,#5260,#5261,#5262));
#1510=EDGE_LOOP('',(#5263,#5264,#5265,#5266));
#1511=EDGE_LOOP('',(#5267,#5268,#5269,#5270));
#1512=EDGE_LOOP('',(#5271,#5272,#5273,#5274));
#1513=EDGE_LOOP('',(#5275,#5276,#5277,#5278));
#1514=EDGE_LOOP('',(#5279,#5280,#5281,#5282));
#1515=EDGE_LOOP('',(#5283,#5284,#5285,#5286));
#1516=EDGE_LOOP('',(#5287,#5288,#5289,#5290));
#1517=EDGE_LOOP('',(#5291,#5292,#5293,#5294));
#1518=EDGE_LOOP('',(#5295,#5296,#5297,#5298));
#1519=EDGE_LOOP('',(#5299,#5300,#5301,#5302));
#1520=EDGE_LOOP('',(#5303,#5304,#5305,#5306));
#1521=EDGE_LOOP('',(#5307,#5308,#5309,#5310));
#1522=EDGE_LOOP('',(#5311,#5312,#5313,#5314));
#1523=EDGE_LOOP('',(#5315,#5316,#5317,#5318));
#1524=EDGE_LOOP('',(#5319,#5320,#5321,#5322));
#1525=EDGE_LOOP('',(#5323,#5324,#5325,#5326));
#1526=EDGE_LOOP('',(#5327,#5328,#5329,#5330));
#1527=EDGE_LOOP('',(#5331,#5332,#5333,#5334));
#1528=EDGE_LOOP('',(#5335));
#1529=EDGE_LOOP('',(#5336));
#1530=EDGE_LOOP('',(#5337,#5338,#5339,#5340));
#1531=EDGE_LOOP('',(#5341));
#1532=EDGE_LOOP('',(#5342));
#1533=EDGE_LOOP('',(#5343,#5344,#5345,#5346));
#1534=EDGE_LOOP('',(#5347,#5348,#5349,#5350));
#1535=EDGE_LOOP('',(#5351,#5352,#5353,#5354));
#1536=EDGE_LOOP('',(#5355,#5356,#5357,#5358));
#1537=EDGE_LOOP('',(#5359,#5360,#5361,#5362));
#1538=EDGE_LOOP('',(#5363,#5364,#5365,#5366));
#1539=EDGE_LOOP('',(#5367,#5368,#5369,#5370));
#1540=EDGE_LOOP('',(#5371));
#1541=EDGE_LOOP('',(#5372));
#1542=EDGE_LOOP('',(#5373,#5374,#5375,#5376));
#1543=EDGE_LOOP('',(#5377));
#1544=EDGE_LOOP('',(#5378));
#1545=EDGE_LOOP('',(#5379,#5380,#5381,#5382));
#1546=EDGE_LOOP('',(#5383,#5384,#5385,#5386));
#1547=EDGE_LOOP('',(#5387,#5388,#5389,#5390));
#1548=EDGE_LOOP('',(#5391,#5392,#5393,#5394));
#1549=EDGE_LOOP('',(#5395,#5396,#5397,#5398));
#1550=EDGE_LOOP('',(#5399,#5400,#5401,#5402));
#1551=EDGE_LOOP('',(#5403,#5404,#5405,#5406));
#1552=EDGE_LOOP('',(#5407,#5408,#5409,#5410));
#1553=EDGE_LOOP('',(#5411,#5412,#5413,#5414));
#1554=EDGE_LOOP('',(#5415,#5416,#5417,#5418));
#1555=EDGE_LOOP('',(#5419,#5420,#5421,#5422));
#1556=EDGE_LOOP('',(#5423,#5424,#5425,#5426));
#1557=EDGE_LOOP('',(#5427,#5428,#5429,#5430));
#1558=EDGE_LOOP('',(#5431,#5432,#5433,#5434));
#1559=EDGE_LOOP('',(#5435,#5436));
#1560=EDGE_LOOP('',(#5437));
#1561=EDGE_LOOP('',(#5438,#5439,#5440,#5441));
#1562=EDGE_LOOP('',(#5442,#5443,#5444,#5445));
#1563=EDGE_LOOP('',(#5446,#5447));
#1564=EDGE_LOOP('',(#5448));
#1565=EDGE_LOOP('',(#5449,#5450,#5451,#5452));
#1566=EDGE_LOOP('',(#5453,#5454,#5455,#5456));
#1567=EDGE_LOOP('',(#5457,#5458,#5459,#5460));
#1568=EDGE_LOOP('',(#5461,#5462,#5463,#5464));
#1569=EDGE_LOOP('',(#5465,#5466,#5467,#5468));
#1570=EDGE_LOOP('',(#5469,#5470,#5471,#5472));
#1571=EDGE_LOOP('',(#5473,#5474,#5475,#5476,#5477,#5478,#5479,#5480,#5481,
#5482));
#1572=EDGE_LOOP('',(#5483,#5484,#5485,#5486));
#1573=EDGE_LOOP('',(#5487,#5488,#5489,#5490,#5491,#5492,#5493,#5494,#5495,
#5496));
#1574=EDGE_LOOP('',(#5497,#5498,#5499,#5500));
#1575=EDGE_LOOP('',(#5501));
#1576=EDGE_LOOP('',(#5502));
#1577=EDGE_LOOP('',(#5503,#5504,#5505,#5506));
#1578=EDGE_LOOP('',(#5507,#5508,#5509,#5510));
#1579=EDGE_LOOP('',(#5511,#5512,#5513,#5514));
#1580=EDGE_LOOP('',(#5515,#5516,#5517,#5518));
#1581=EDGE_LOOP('',(#5519,#5520,#5521,#5522));
#1582=EDGE_LOOP('',(#5523,#5524,#5525,#5526));
#1583=EDGE_LOOP('',(#5527,#5528,#5529,#5530));
#1584=EDGE_LOOP('',(#5531,#5532,#5533,#5534));
#1585=EDGE_LOOP('',(#5535,#5536));
#1586=EDGE_LOOP('',(#5537));
#1587=EDGE_LOOP('',(#5538,#5539,#5540,#5541));
#1588=EDGE_LOOP('',(#5542,#5543,#5544,#5545));
#1589=EDGE_LOOP('',(#5546,#5547));
#1590=EDGE_LOOP('',(#5548));
#1591=EDGE_LOOP('',(#5549,#5550,#5551,#5552));
#1592=EDGE_LOOP('',(#5553,#5554,#5555,#5556));
#1593=EDGE_LOOP('',(#5557,#5558,#5559,#5560));
#1594=EDGE_LOOP('',(#5561,#5562,#5563,#5564));
#1595=EDGE_LOOP('',(#5565,#5566,#5567,#5568));
#1596=EDGE_LOOP('',(#5569,#5570,#5571,#5572));
#1597=EDGE_LOOP('',(#5573,#5574,#5575,#5576,#5577,#5578,#5579,#5580,#5581,
#5582));
#1598=EDGE_LOOP('',(#5583,#5584,#5585,#5586));
#1599=EDGE_LOOP('',(#5587,#5588,#5589,#5590,#5591,#5592,#5593,#5594,#5595,
#5596));
#1600=EDGE_LOOP('',(#5597,#5598,#5599,#5600));
#1601=EDGE_LOOP('',(#5601));
#1602=EDGE_LOOP('',(#5602));
#1603=EDGE_LOOP('',(#5603,#5604,#5605,#5606));
#1604=EDGE_LOOP('',(#5607,#5608,#5609,#5610));
#1605=EDGE_LOOP('',(#5611,#5612,#5613,#5614));
#1606=EDGE_LOOP('',(#5615,#5616,#5617,#5618));
#1607=EDGE_LOOP('',(#5619,#5620,#5621,#5622));
#1608=EDGE_LOOP('',(#5623,#5624,#5625,#5626));
#1609=EDGE_LOOP('',(#5627,#5628,#5629,#5630));
#1610=EDGE_LOOP('',(#5631,#5632,#5633,#5634));
#1611=EDGE_LOOP('',(#5635,#5636,#5637,#5638));
#1612=EDGE_LOOP('',(#5639,#5640,#5641,#5642));
#1613=EDGE_LOOP('',(#5643,#5644,#5645,#5646));
#1614=EDGE_LOOP('',(#5647,#5648,#5649,#5650));
#1615=EDGE_LOOP('',(#5651,#5652,#5653,#5654));
#1616=EDGE_LOOP('',(#5655,#5656,#5657,#5658));
#1617=EDGE_LOOP('',(#5659,#5660,#5661,#5662));
#1618=EDGE_LOOP('',(#5663,#5664,#5665,#5666));
#1619=EDGE_LOOP('',(#5667,#5668,#5669,#5670));
#1620=EDGE_LOOP('',(#5671,#5672,#5673,#5674));
#1621=EDGE_LOOP('',(#5675,#5676,#5677,#5678));
#1622=EDGE_LOOP('',(#5679,#5680,#5681,#5682));
#1623=EDGE_LOOP('',(#5683,#5684,#5685,#5686));
#1624=EDGE_LOOP('',(#5687,#5688,#5689,#5690));
#1625=EDGE_LOOP('',(#5691,#5692,#5693,#5694));
#1626=EDGE_LOOP('',(#5695,#5696,#5697,#5698));
#1627=EDGE_LOOP('',(#5699,#5700,#5701,#5702));
#1628=EDGE_LOOP('',(#5703,#5704,#5705,#5706));
#1629=EDGE_LOOP('',(#5707,#5708,#5709,#5710));
#1630=EDGE_LOOP('',(#5711,#5712,#5713,#5714));
#1631=EDGE_LOOP('',(#5715,#5716,#5717,#5718));
#1632=EDGE_LOOP('',(#5719,#5720,#5721,#5722));
#1633=EDGE_LOOP('',(#5723,#5724,#5725,#5726));
#1634=EDGE_LOOP('',(#5727,#5728,#5729,#5730));
#1635=EDGE_LOOP('',(#5731,#5732,#5733,#5734));
#1636=EDGE_LOOP('',(#5735,#5736,#5737,#5738));
#1637=EDGE_LOOP('',(#5739,#5740,#5741,#5742));
#1638=EDGE_LOOP('',(#5743,#5744,#5745,#5746));
#1639=EDGE_LOOP('',(#5747,#5748,#5749,#5750));
#1640=EDGE_LOOP('',(#5751,#5752,#5753,#5754));
#1641=EDGE_LOOP('',(#5755,#5756,#5757,#5758));
#1642=EDGE_LOOP('',(#5759,#5760,#5761,#5762));
#1643=EDGE_LOOP('',(#5763,#5764,#5765,#5766));
#1644=EDGE_LOOP('',(#5767,#5768,#5769,#5770));
#1645=EDGE_LOOP('',(#5771,#5772,#5773,#5774));
#1646=EDGE_LOOP('',(#5775,#5776,#5777,#5778));
#1647=EDGE_LOOP('',(#5779,#5780,#5781,#5782));
#1648=EDGE_LOOP('',(#5783,#5784,#5785,#5786));
#1649=EDGE_LOOP('',(#5787,#5788,#5789,#5790));
#1650=EDGE_LOOP('',(#5791,#5792,#5793,#5794));
#1651=EDGE_LOOP('',(#5795,#5796,#5797,#5798));
#1652=EDGE_LOOP('',(#5799,#5800,#5801,#5802));
#1653=EDGE_LOOP('',(#5803,#5804,#5805,#5806));
#1654=EDGE_LOOP('',(#5807,#5808,#5809,#5810,#5811,#5812,#5813,#5814,#5815,
#5816,#5817,#5818,#5819,#5820,#5821,#5822,#5823,#5824,#5825,#5826,#5827,
#5828,#5829,#5830,#5831,#5832,#5833,#5834,#5835,#5836,#5837,#5838,#5839,
#5840,#5841,#5842,#5843,#5844,#5845,#5846,#5847,#5848,#5849,#5850));
#1655=EDGE_LOOP('',(#5851));
#1656=EDGE_LOOP('',(#5852,#5853,#5854,#5855,#5856,#5857,#5858,#5859,#5860,
#5861,#5862,#5863,#5864,#5865,#5866,#5867,#5868,#5869,#5870,#5871,#5872,
#5873,#5874,#5875,#5876,#5877,#5878,#5879,#5880,#5881,#5882,#5883,#5884,
#5885,#5886,#5887,#5888,#5889,#5890,#5891,#5892,#5893,#5894,#5895));
#1657=EDGE_LOOP('',(#5896));
#1658=EDGE_LOOP('',(#5897,#5898,#5899,#5900));
#1659=EDGE_LOOP('',(#5901));
#1660=EDGE_LOOP('',(#5902));
#1661=EDGE_LOOP('',(#5903,#5904,#5905,#5906));
#1662=EDGE_LOOP('',(#5907));
#1663=EDGE_LOOP('',(#5908));
#1664=EDGE_LOOP('',(#5909,#5910,#5911,#5912));
#1665=EDGE_LOOP('',(#5913));
#1666=EDGE_LOOP('',(#5914));
#1667=EDGE_LOOP('',(#5915,#5916,#5917,#5918));
#1668=EDGE_LOOP('',(#5919));
#1669=EDGE_LOOP('',(#5920));
#1670=EDGE_LOOP('',(#5921,#5922,#5923,#5924));
#1671=EDGE_LOOP('',(#5925,#5926,#5927,#5928));
#1672=EDGE_LOOP('',(#5929,#5930,#5931,#5932));
#1673=EDGE_LOOP('',(#5933,#5934,#5935,#5936));
#1674=EDGE_LOOP('',(#5937,#5938,#5939,#5940));
#1675=EDGE_LOOP('',(#5941,#5942,#5943,#5944));
#1676=EDGE_LOOP('',(#5945,#5946,#5947,#5948));
#1677=EDGE_LOOP('',(#5949,#5950,#5951,#5952));
#1678=EDGE_LOOP('',(#5953,#5954,#5955,#5956));
#1679=EDGE_LOOP('',(#5957));
#1680=EDGE_LOOP('',(#5958));
#1681=EDGE_LOOP('',(#5959));
#1682=EDGE_LOOP('',(#5960));
#1683=EDGE_LOOP('',(#5961,#5962,#5963,#5964));
#1684=EDGE_LOOP('',(#5965,#5966,#5967,#5968));
#1685=EDGE_LOOP('',(#5969,#5970,#5971,#5972));
#1686=EDGE_LOOP('',(#5973,#5974,#5975,#5976));
#1687=EDGE_LOOP('',(#5977,#5978,#5979,#5980));
#1688=EDGE_LOOP('',(#5981,#5982,#5983,#5984));
#1689=EDGE_LOOP('',(#5985));
#1690=EDGE_LOOP('',(#5986));
#1691=EDGE_LOOP('',(#5987));
#1692=EDGE_LOOP('',(#5988));
#1693=EDGE_LOOP('',(#5989,#5990,#5991,#5992));
#1694=EDGE_LOOP('',(#5993,#5994,#5995,#5996,#5997,#5998,#5999,#6000,#6001,
#6002,#6003,#6004));
#1695=EDGE_LOOP('',(#6005,#6006,#6007,#6008,#6009,#6010,#6011,#6012,#6013,
#6014,#6015,#6016));
#1696=EDGE_LOOP('',(#6017));
#1697=EDGE_LOOP('',(#6018,#6019,#6020,#6021));
#1698=EDGE_LOOP('',(#6022,#6023,#6024,#6025));
#1699=EDGE_LOOP('',(#6026,#6027,#6028,#6029));
#1700=EDGE_LOOP('',(#6030));
#1701=EDGE_LOOP('',(#6031));
#1702=EDGE_LOOP('',(#6032,#6033,#6034,#6035));
#1703=EDGE_LOOP('',(#6036,#6037,#6038,#6039));
#1704=EDGE_LOOP('',(#6040,#6041,#6042,#6043));
#1705=EDGE_LOOP('',(#6044));
#1706=EDGE_LOOP('',(#6045,#6046,#6047,#6048));
#1707=EDGE_LOOP('',(#6049,#6050,#6051,#6052));
#1708=EDGE_LOOP('',(#6053,#6054,#6055,#6056));
#1709=EDGE_LOOP('',(#6057,#6058,#6059,#6060));
#1710=EDGE_LOOP('',(#6061,#6062,#6063,#6064));
#1711=EDGE_LOOP('',(#6065,#6066,#6067,#6068));
#1712=EDGE_LOOP('',(#6069,#6070,#6071,#6072,#6073,#6074));
#1713=EDGE_LOOP('',(#6075,#6076,#6077,#6078,#6079,#6080));
#1714=EDGE_LOOP('',(#6081,#6082,#6083,#6084));
#1715=EDGE_LOOP('',(#6085,#6086,#6087,#6088));
#1716=EDGE_LOOP('',(#6089,#6090,#6091,#6092));
#1717=EDGE_LOOP('',(#6093));
#1718=EDGE_LOOP('',(#6094,#6095,#6096,#6097,#6098,#6099,#6100,#6101,#6102,
#6103));
#1719=EDGE_LOOP('',(#6104,#6105,#6106,#6107));
#1720=EDGE_LOOP('',(#6108,#6109,#6110,#6111));
#1721=EDGE_LOOP('',(#6112,#6113,#6114,#6115,#6116,#6117,#6118,#6119,#6120,
#6121));
#1722=EDGE_LOOP('',(#6122,#6123,#6124,#6125));
#1723=EDGE_LOOP('',(#6126,#6127,#6128,#6129,#6130,#6131));
#1724=EDGE_LOOP('',(#6132,#6133,#6134,#6135,#6136,#6137,#6138,#6139));
#1725=EDGE_LOOP('',(#6140,#6141,#6142,#6143,#6144));
#1726=EDGE_LOOP('',(#6145,#6146,#6147,#6148));
#1727=EDGE_LOOP('',(#6149,#6150,#6151,#6152,#6153,#6154));
#1728=EDGE_LOOP('',(#6155,#6156,#6157,#6158));
#1729=EDGE_LOOP('',(#6159,#6160,#6161,#6162));
#1730=EDGE_LOOP('',(#6163,#6164,#6165,#6166));
#1731=EDGE_LOOP('',(#6167,#6168,#6169,#6170));
#1732=EDGE_LOOP('',(#6171,#6172,#6173,#6174));
#1733=EDGE_LOOP('',(#6175,#6176,#6177,#6178));
#1734=EDGE_LOOP('',(#6179,#6180,#6181,#6182));
#1735=EDGE_LOOP('',(#6183,#6184,#6185,#6186,#6187,#6188));
#1736=EDGE_LOOP('',(#6189,#6190,#6191,#6192,#6193,#6194));
#1737=EDGE_LOOP('',(#6195));
#1738=EDGE_LOOP('',(#6196));
#1739=EDGE_LOOP('',(#6197,#6198,#6199,#6200));
#1740=EDGE_LOOP('',(#6201,#6202,#6203,#6204));
#1741=EDGE_LOOP('',(#6205,#6206,#6207,#6208));
#1742=EDGE_LOOP('',(#6209));
#1743=EDGE_LOOP('',(#6210));
#1744=EDGE_LOOP('',(#6211,#6212,#6213,#6214));
#1745=EDGE_LOOP('',(#6215,#6216,#6217,#6218));
#1746=EDGE_LOOP('',(#6219,#6220,#6221,#6222));
#1747=EDGE_LOOP('',(#6223,#6224,#6225,#6226));
#1748=EDGE_LOOP('',(#6227,#6228,#6229,#6230));
#1749=EDGE_LOOP('',(#6231,#6232,#6233,#6234));
#1750=EDGE_LOOP('',(#6235,#6236,#6237,#6238));
#1751=EDGE_LOOP('',(#6239,#6240,#6241,#6242));
#1752=EDGE_LOOP('',(#6243,#6244,#6245,#6246));
#1753=EDGE_LOOP('',(#6247,#6248,#6249,#6250));
#1754=EDGE_LOOP('',(#6251,#6252,#6253,#6254));
#1755=EDGE_LOOP('',(#6255,#6256,#6257,#6258));
#1756=EDGE_LOOP('',(#6259,#6260,#6261,#6262));
#1757=EDGE_LOOP('',(#6263,#6264,#6265,#6266));
#1758=EDGE_LOOP('',(#6267,#6268,#6269,#6270));
#1759=EDGE_LOOP('',(#6271,#6272,#6273,#6274));
#1760=EDGE_LOOP('',(#6275,#6276,#6277,#6278));
#1761=EDGE_LOOP('',(#6279,#6280,#6281,#6282));
#1762=EDGE_LOOP('',(#6283,#6284,#6285,#6286));
#1763=EDGE_LOOP('',(#6287,#6288,#6289,#6290));
#1764=EDGE_LOOP('',(#6291,#6292,#6293,#6294));
#1765=EDGE_LOOP('',(#6295,#6296,#6297,#6298));
#1766=EDGE_LOOP('',(#6299,#6300,#6301,#6302));
#1767=EDGE_LOOP('',(#6303,#6304,#6305,#6306));
#1768=EDGE_LOOP('',(#6307,#6308,#6309,#6310));
#1769=EDGE_LOOP('',(#6311,#6312,#6313,#6314));
#1770=EDGE_LOOP('',(#6315));
#1771=EDGE_LOOP('',(#6316));
#1772=EDGE_LOOP('',(#6317));
#1773=EDGE_LOOP('',(#6318));
#1774=EDGE_LOOP('',(#6319));
#1775=EDGE_LOOP('',(#6320));
#1776=EDGE_LOOP('',(#6321));
#1777=EDGE_LOOP('',(#6322));
#1778=EDGE_LOOP('',(#6323));
#1779=EDGE_LOOP('',(#6324));
#1780=EDGE_LOOP('',(#6325));
#1781=EDGE_LOOP('',(#6326));
#1782=EDGE_LOOP('',(#6327));
#1783=EDGE_LOOP('',(#6328));
#1784=EDGE_LOOP('',(#6329));
#1785=EDGE_LOOP('',(#6330));
#1786=EDGE_LOOP('',(#6331));
#1787=EDGE_LOOP('',(#6332));
#1788=EDGE_LOOP('',(#6333));
#1789=EDGE_LOOP('',(#6334,#6335,#6336,#6337));
#1790=EDGE_LOOP('',(#6338));
#1791=EDGE_LOOP('',(#6339));
#1792=EDGE_LOOP('',(#6340));
#1793=EDGE_LOOP('',(#6341));
#1794=EDGE_LOOP('',(#6342));
#1795=EDGE_LOOP('',(#6343));
#1796=EDGE_LOOP('',(#6344));
#1797=EDGE_LOOP('',(#6345));
#1798=EDGE_LOOP('',(#6346));
#1799=EDGE_LOOP('',(#6347));
#1800=EDGE_LOOP('',(#6348));
#1801=EDGE_LOOP('',(#6349));
#1802=EDGE_LOOP('',(#6350));
#1803=EDGE_LOOP('',(#6351));
#1804=EDGE_LOOP('',(#6352));
#1805=EDGE_LOOP('',(#6353));
#1806=EDGE_LOOP('',(#6354));
#1807=EDGE_LOOP('',(#6355));
#1808=EDGE_LOOP('',(#6356));
#1809=EDGE_LOOP('',(#6357,#6358,#6359,#6360));
#1810=EDGE_LOOP('',(#6361,#6362,#6363,#6364));
#1811=EDGE_LOOP('',(#6365));
#1812=EDGE_LOOP('',(#6366));
#1813=EDGE_LOOP('',(#6367));
#1814=EDGE_LOOP('',(#6368));
#1815=EDGE_LOOP('',(#6369,#6370,#6371,#6372));
#1816=EDGE_LOOP('',(#6373,#6374,#6375,#6376));
#1817=EDGE_LOOP('',(#6377,#6378,#6379,#6380));
#1818=EDGE_LOOP('',(#6381));
#1819=EDGE_LOOP('',(#6382));
#1820=EDGE_LOOP('',(#6383,#6384,#6385,#6386));
#1821=EDGE_LOOP('',(#6387,#6388,#6389,#6390));
#1822=EDGE_LOOP('',(#6391,#6392,#6393,#6394));
#1823=EDGE_LOOP('',(#6395,#6396,#6397,#6398));
#1824=EDGE_LOOP('',(#6399));
#1825=EDGE_LOOP('',(#6400));
#1826=EDGE_LOOP('',(#6401,#6402,#6403,#6404));
#1827=EDGE_LOOP('',(#6405,#6406,#6407,#6408,#6409,#6410));
#1828=EDGE_LOOP('',(#6411,#6412,#6413,#6414,#6415,#6416));
#1829=EDGE_LOOP('',(#6417,#6418));
#1830=EDGE_LOOP('',(#6419,#6420,#6421,#6422,#6423,#6424,#6425,#6426));
#1831=EDGE_LOOP('',(#6427,#6428));
#1832=EDGE_LOOP('',(#6429,#6430,#6431,#6432,#6433,#6434,#6435,#6436));
#1833=EDGE_LOOP('',(#6437,#6438));
#1834=EDGE_LOOP('',(#6439,#6440,#6441,#6442,#6443,#6444,#6445,#6446));
#1835=EDGE_LOOP('',(#6447,#6448));
#1836=EDGE_LOOP('',(#6449,#6450,#6451,#6452,#6453,#6454,#6455,#6456));
#1837=EDGE_LOOP('',(#6457,#6458,#6459,#6460,#6461,#6462,#6463,#6464,#6465,
#6466,#6467,#6468));
#1838=EDGE_LOOP('',(#6469,#6470,#6471,#6472,#6473,#6474,#6475,#6476,#6477,
#6478,#6479,#6480));
#1839=EDGE_LOOP('',(#6481,#6482,#6483,#6484,#6485,#6486,#6487,#6488,#6489,
#6490,#6491,#6492));
#1840=EDGE_LOOP('',(#6493,#6494,#6495,#6496,#6497,#6498,#6499,#6500,#6501,
#6502));
#1841=EDGE_LOOP('',(#6503,#6504,#6505,#6506));
#1842=EDGE_LOOP('',(#6507,#6508,#6509,#6510));
#1843=EDGE_LOOP('',(#6511));
#1844=EDGE_LOOP('',(#6512));
#1845=EDGE_LOOP('',(#6513));
#1846=EDGE_LOOP('',(#6514));
#1847=EDGE_LOOP('',(#6515,#6516,#6517,#6518));
#1848=EDGE_LOOP('',(#6519,#6520,#6521,#6522,#6523,#6524,#6525,#6526,#6527,
#6528));
#1849=EDGE_LOOP('',(#6529,#6530,#6531,#6532));
#1850=EDGE_LOOP('',(#6533,#6534,#6535,#6536));
#1851=EDGE_LOOP('',(#6537,#6538,#6539,#6540));
#1852=EDGE_LOOP('',(#6541,#6542,#6543,#6544));
#1853=EDGE_LOOP('',(#6545,#6546,#6547,#6548));
#1854=EDGE_LOOP('',(#6549,#6550,#6551,#6552,#6553,#6554,#6555,#6556,#6557,
#6558,#6559,#6560));
#1855=EDGE_LOOP('',(#6561,#6562,#6563,#6564));
#1856=EDGE_LOOP('',(#6565,#6566,#6567,#6568));
#1857=EDGE_LOOP('',(#6569,#6570,#6571,#6572));
#1858=EDGE_LOOP('',(#6573,#6574,#6575,#6576));
#1859=EDGE_LOOP('',(#6577,#6578,#6579,#6580));
#1860=EDGE_LOOP('',(#6581,#6582,#6583,#6584));
#1861=EDGE_LOOP('',(#6585,#6586,#6587,#6588));
#1862=EDGE_LOOP('',(#6589,#6590,#6591,#6592));
#1863=EDGE_LOOP('',(#6593,#6594,#6595,#6596,#6597,#6598,#6599,#6600));
#1864=EDGE_LOOP('',(#6601,#6602,#6603,#6604,#6605,#6606,#6607,#6608));
#1865=EDGE_LOOP('',(#6609,#6610,#6611,#6612));
#1866=EDGE_LOOP('',(#6613,#6614,#6615,#6616));
#1867=EDGE_LOOP('',(#6617,#6618,#6619,#6620));
#1868=EDGE_LOOP('',(#6621,#6622,#6623,#6624));
#1869=EDGE_LOOP('',(#6625,#6626,#6627,#6628));
#1870=EDGE_LOOP('',(#6629,#6630,#6631,#6632));
#1871=EDGE_LOOP('',(#6633,#6634,#6635,#6636));
#1872=EDGE_LOOP('',(#6637,#6638,#6639,#6640));
#1873=EDGE_LOOP('',(#6641,#6642,#6643,#6644,#6645,#6646,#6647,#6648));
#1874=EDGE_LOOP('',(#6649,#6650,#6651,#6652,#6653,#6654,#6655,#6656));
#1875=EDGE_LOOP('',(#6657,#6658,#6659,#6660));
#1876=EDGE_LOOP('',(#6661,#6662,#6663,#6664));
#1877=EDGE_LOOP('',(#6665));
#1878=EDGE_LOOP('',(#6666));
#1879=EDGE_LOOP('',(#6667,#6668,#6669,#6670));
#1880=EDGE_LOOP('',(#6671));
#1881=EDGE_LOOP('',(#6672));
#1882=EDGE_LOOP('',(#6673));
#1883=EDGE_LOOP('',(#6674,#6675,#6676,#6677));
#1884=EDGE_LOOP('',(#6678,#6679,#6680,#6681));
#1885=EDGE_LOOP('',(#6682,#6683,#6684,#6685));
#1886=EDGE_LOOP('',(#6686));
#1887=EDGE_LOOP('',(#6687));
#1888=EDGE_LOOP('',(#6688,#6689,#6690,#6691));
#1889=EDGE_LOOP('',(#6692,#6693,#6694,#6695));
#1890=EDGE_LOOP('',(#6696,#6697,#6698,#6699));
#1891=EDGE_LOOP('',(#6700));
#1892=EDGE_LOOP('',(#6701,#6702,#6703,#6704));
#1893=EDGE_LOOP('',(#6705,#6706,#6707,#6708));
#1894=EDGE_LOOP('',(#6709,#6710,#6711,#6712));
#1895=EDGE_LOOP('',(#6713,#6714,#6715,#6716));
#1896=EDGE_LOOP('',(#6717,#6718,#6719,#6720));
#1897=EDGE_LOOP('',(#6721,#6722,#6723,#6724));
#1898=EDGE_LOOP('',(#6725,#6726,#6727,#6728,#6729,#6730));
#1899=EDGE_LOOP('',(#6731,#6732,#6733,#6734,#6735,#6736));
#1900=EDGE_LOOP('',(#6737,#6738,#6739,#6740));
#1901=EDGE_LOOP('',(#6741,#6742,#6743,#6744));
#1902=EDGE_LOOP('',(#6745));
#1903=EDGE_LOOP('',(#6746));
#1904=EDGE_LOOP('',(#6747));
#1905=EDGE_LOOP('',(#6748));
#1906=EDGE_LOOP('',(#6749));
#1907=EDGE_LOOP('',(#6750,#6751,#6752,#6753));
#1908=EDGE_LOOP('',(#6754,#6755,#6756,#6757));
#1909=EDGE_LOOP('',(#6758,#6759,#6760,#6761));
#1910=EDGE_LOOP('',(#6762));
#1911=EDGE_LOOP('',(#6763));
#1912=EDGE_LOOP('',(#6764,#6765,#6766,#6767));
#1913=EDGE_LOOP('',(#6768,#6769,#6770,#6771));
#1914=EDGE_LOOP('',(#6772,#6773,#6774,#6775));
#1915=EDGE_LOOP('',(#6776));
#1916=EDGE_LOOP('',(#6777,#6778,#6779,#6780));
#1917=EDGE_LOOP('',(#6781,#6782,#6783,#6784));
#1918=EDGE_LOOP('',(#6785,#6786,#6787,#6788));
#1919=EDGE_LOOP('',(#6789,#6790,#6791,#6792));
#1920=EDGE_LOOP('',(#6793,#6794,#6795,#6796));
#1921=EDGE_LOOP('',(#6797,#6798,#6799,#6800));
#1922=EDGE_LOOP('',(#6801,#6802,#6803,#6804,#6805,#6806));
#1923=EDGE_LOOP('',(#6807,#6808,#6809,#6810,#6811,#6812));
#1924=EDGE_LOOP('',(#6813,#6814,#6815,#6816));
#1925=EDGE_LOOP('',(#6817,#6818,#6819,#6820));
#1926=EDGE_LOOP('',(#6821));
#1927=EDGE_LOOP('',(#6822));
#1928=EDGE_LOOP('',(#6823,#6824,#6825,#6826));
#1929=EDGE_LOOP('',(#6827));
#1930=EDGE_LOOP('',(#6828));
#1931=EDGE_LOOP('',(#6829,#6830,#6831,#6832));
#1932=EDGE_LOOP('',(#6833,#6834,#6835,#6836));
#1933=EDGE_LOOP('',(#6837,#6838,#6839,#6840));
#1934=EDGE_LOOP('',(#6841,#6842,#6843,#6844));
#1935=EDGE_LOOP('',(#6845,#6846,#6847,#6848));
#1936=EDGE_LOOP('',(#6849,#6850,#6851,#6852));
#1937=EDGE_LOOP('',(#6853,#6854,#6855,#6856,#6857,#6858));
#1938=EDGE_LOOP('',(#6859,#6860,#6861,#6862,#6863,#6864));
#1939=EDGE_LOOP('',(#6865));
#1940=EDGE_LOOP('',(#6866));
#1941=EDGE_LOOP('',(#6867,#6868,#6869,#6870));
#1942=EDGE_LOOP('',(#6871,#6872,#6873,#6874));
#1943=EDGE_LOOP('',(#6875,#6876,#6877,#6878));
#1944=EDGE_LOOP('',(#6879));
#1945=EDGE_LOOP('',(#6880));
#1946=EDGE_LOOP('',(#6881,#6882,#6883,#6884));
#1947=EDGE_LOOP('',(#6885,#6886,#6887,#6888));
#1948=LINE('',#10695,#2657);
#1949=LINE('',#10701,#2658);
#1950=LINE('',#10707,#2659);
#1951=LINE('',#10713,#2660);
#1952=LINE('',#10719,#2661);
#1953=LINE('',#10725,#2662);
#1954=LINE('',#10730,#2663);
#1955=LINE('',#10732,#2664);
#1956=LINE('',#10734,#2665);
#1957=LINE('',#10735,#2666);
#1958=LINE('',#10738,#2667);
#1959=LINE('',#10740,#2668);
#1960=LINE('',#10741,#2669);
#1961=LINE('',#10744,#2670);
#1962=LINE('',#10746,#2671);
#1963=LINE('',#10747,#2672);
#1964=LINE('',#10749,#2673);
#1965=LINE('',#10750,#2674);
#1966=LINE('',#10758,#2675);
#1967=LINE('',#10764,#2676);
#1968=LINE('',#10770,#2677);
#1969=LINE('',#10776,#2678);
#1970=LINE('',#10782,#2679);
#1971=LINE('',#10788,#2680);
#1972=LINE('',#10793,#2681);
#1973=LINE('',#10795,#2682);
#1974=LINE('',#10797,#2683);
#1975=LINE('',#10798,#2684);
#1976=LINE('',#10801,#2685);
#1977=LINE('',#10803,#2686);
#1978=LINE('',#10804,#2687);
#1979=LINE('',#10807,#2688);
#1980=LINE('',#10809,#2689);
#1981=LINE('',#10810,#2690);
#1982=LINE('',#10812,#2691);
#1983=LINE('',#10813,#2692);
#1984=LINE('',#10821,#2693);
#1985=LINE('',#10827,#2694);
#1986=LINE('',#10832,#2695);
#1987=LINE('',#10834,#2696);
#1988=LINE('',#10836,#2697);
#1989=LINE('',#10837,#2698);
#1990=LINE('',#10840,#2699);
#1991=LINE('',#10842,#2700);
#1992=LINE('',#10843,#2701);
#1993=LINE('',#10846,#2702);
#1994=LINE('',#10848,#2703);
#1995=LINE('',#10849,#2704);
#1996=LINE('',#10851,#2705);
#1997=LINE('',#10852,#2706);
#1998=LINE('',#10860,#2707);
#1999=LINE('',#10866,#2708);
#2000=LINE('',#10871,#2709);
#2001=LINE('',#10873,#2710);
#2002=LINE('',#10875,#2711);
#2003=LINE('',#10876,#2712);
#2004=LINE('',#10879,#2713);
#2005=LINE('',#10881,#2714);
#2006=LINE('',#10882,#2715);
#2007=LINE('',#10885,#2716);
#2008=LINE('',#10887,#2717);
#2009=LINE('',#10888,#2718);
#2010=LINE('',#10890,#2719);
#2011=LINE('',#10891,#2720);
#2012=LINE('',#10898,#2721);
#2013=LINE('',#10900,#2722);
#2014=LINE('',#10902,#2723);
#2015=LINE('',#10903,#2724);
#2016=LINE('',#10906,#2725);
#2017=LINE('',#10908,#2726);
#2018=LINE('',#10909,#2727);
#2019=LINE('',#10912,#2728);
#2020=LINE('',#10914,#2729);
#2021=LINE('',#10915,#2730);
#2022=LINE('',#10917,#2731);
#2023=LINE('',#10918,#2732);
#2024=LINE('',#10925,#2733);
#2025=LINE('',#10927,#2734);
#2026=LINE('',#10929,#2735);
#2027=LINE('',#10930,#2736);
#2028=LINE('',#10933,#2737);
#2029=LINE('',#10935,#2738);
#2030=LINE('',#10936,#2739);
#2031=LINE('',#10939,#2740);
#2032=LINE('',#10941,#2741);
#2033=LINE('',#10942,#2742);
#2034=LINE('',#10944,#2743);
#2035=LINE('',#10945,#2744);
#2036=LINE('',#10953,#2745);
#2037=LINE('',#10959,#2746);
#2038=LINE('',#10964,#2747);
#2039=LINE('',#10966,#2748);
#2040=LINE('',#10968,#2749);
#2041=LINE('',#10969,#2750);
#2042=LINE('',#10972,#2751);
#2043=LINE('',#10974,#2752);
#2044=LINE('',#10975,#2753);
#2045=LINE('',#10978,#2754);
#2046=LINE('',#10980,#2755);
#2047=LINE('',#10981,#2756);
#2048=LINE('',#10983,#2757);
#2049=LINE('',#10984,#2758);
#2050=LINE('',#10992,#2759);
#2051=LINE('',#10998,#2760);
#2052=LINE('',#11003,#2761);
#2053=LINE('',#11005,#2762);
#2054=LINE('',#11007,#2763);
#2055=LINE('',#11008,#2764);
#2056=LINE('',#11011,#2765);
#2057=LINE('',#11013,#2766);
#2058=LINE('',#11014,#2767);
#2059=LINE('',#11017,#2768);
#2060=LINE('',#11019,#2769);
#2061=LINE('',#11020,#2770);
#2062=LINE('',#11022,#2771);
#2063=LINE('',#11023,#2772);
#2064=LINE('',#11030,#2773);
#2065=LINE('',#11032,#2774);
#2066=LINE('',#11034,#2775);
#2067=LINE('',#11035,#2776);
#2068=LINE('',#11038,#2777);
#2069=LINE('',#11040,#2778);
#2070=LINE('',#11041,#2779);
#2071=LINE('',#11044,#2780);
#2072=LINE('',#11046,#2781);
#2073=LINE('',#11047,#2782);
#2074=LINE('',#11049,#2783);
#2075=LINE('',#11050,#2784);
#2076=LINE('',#11057,#2785);
#2077=LINE('',#11059,#2786);
#2078=LINE('',#11061,#2787);
#2079=LINE('',#11062,#2788);
#2080=LINE('',#11065,#2789);
#2081=LINE('',#11067,#2790);
#2082=LINE('',#11068,#2791);
#2083=LINE('',#11071,#2792);
#2084=LINE('',#11073,#2793);
#2085=LINE('',#11074,#2794);
#2086=LINE('',#11076,#2795);
#2087=LINE('',#11077,#2796);
#2088=LINE('',#11084,#2797);
#2089=LINE('',#11088,#2798);
#2090=LINE('',#11091,#2799);
#2091=LINE('',#11093,#2800);
#2092=LINE('',#11101,#2801);
#2093=LINE('',#11105,#2802);
#2094=LINE('',#11108,#2803);
#2095=LINE('',#11110,#2804);
#2096=LINE('',#11117,#2805);
#2097=LINE('',#11119,#2806);
#2098=LINE('',#11120,#2807);
#2099=LINE('',#11122,#2808);
#2100=LINE('',#11123,#2809);
#2101=LINE('',#11126,#2810);
#2102=LINE('',#11128,#2811);
#2103=LINE('',#11129,#2812);
#2104=LINE('',#11133,#2813);
#2105=LINE('',#11137,#2814);
#2106=LINE('',#11141,#2815);
#2107=LINE('',#11142,#2816);
#2108=LINE('',#11143,#2817);
#2109=LINE('',#11146,#2818);
#2110=LINE('',#11147,#2819);
#2111=LINE('',#11150,#2820);
#2112=LINE('',#11151,#2821);
#2113=LINE('',#11153,#2822);
#2114=LINE('',#11159,#2823);
#2115=LINE('',#11161,#2824);
#2116=LINE('',#11163,#2825);
#2117=LINE('',#11164,#2826);
#2118=LINE('',#11167,#2827);
#2119=LINE('',#11169,#2828);
#2120=LINE('',#11170,#2829);
#2121=LINE('',#11173,#2830);
#2122=LINE('',#11175,#2831);
#2123=LINE('',#11176,#2832);
#2124=LINE('',#11178,#2833);
#2125=LINE('',#11179,#2834);
#2126=LINE('',#11186,#2835);
#2127=LINE('',#11190,#2836);
#2128=LINE('',#11193,#2837);
#2129=LINE('',#11195,#2838);
#2130=LINE('',#11203,#2839);
#2131=LINE('',#11207,#2840);
#2132=LINE('',#11210,#2841);
#2133=LINE('',#11212,#2842);
#2134=LINE('',#11219,#2843);
#2135=LINE('',#11221,#2844);
#2136=LINE('',#11222,#2845);
#2137=LINE('',#11224,#2846);
#2138=LINE('',#11225,#2847);
#2139=LINE('',#11228,#2848);
#2140=LINE('',#11230,#2849);
#2141=LINE('',#11231,#2850);
#2142=LINE('',#11235,#2851);
#2143=LINE('',#11239,#2852);
#2144=LINE('',#11243,#2853);
#2145=LINE('',#11244,#2854);
#2146=LINE('',#11245,#2855);
#2147=LINE('',#11248,#2856);
#2148=LINE('',#11249,#2857);
#2149=LINE('',#11252,#2858);
#2150=LINE('',#11253,#2859);
#2151=LINE('',#11255,#2860);
#2152=LINE('',#11261,#2861);
#2153=LINE('',#11263,#2862);
#2154=LINE('',#11265,#2863);
#2155=LINE('',#11266,#2864);
#2156=LINE('',#11269,#2865);
#2157=LINE('',#11271,#2866);
#2158=LINE('',#11272,#2867);
#2159=LINE('',#11275,#2868);
#2160=LINE('',#11277,#2869);
#2161=LINE('',#11278,#2870);
#2162=LINE('',#11280,#2871);
#2163=LINE('',#11281,#2872);
#2164=LINE('',#11288,#2873);
#2165=LINE('',#11290,#2874);
#2166=LINE('',#11292,#2875);
#2167=LINE('',#11293,#2876);
#2168=LINE('',#11296,#2877);
#2169=LINE('',#11298,#2878);
#2170=LINE('',#11299,#2879);
#2171=LINE('',#11302,#2880);
#2172=LINE('',#11304,#2881);
#2173=LINE('',#11305,#2882);
#2174=LINE('',#11308,#2883);
#2175=LINE('',#11310,#2884);
#2176=LINE('',#11311,#2885);
#2177=LINE('',#11314,#2886);
#2178=LINE('',#11316,#2887);
#2179=LINE('',#11317,#2888);
#2180=LINE('',#11320,#2889);
#2181=LINE('',#11322,#2890);
#2182=LINE('',#11323,#2891);
#2183=LINE('',#11326,#2892);
#2184=LINE('',#11328,#2893);
#2185=LINE('',#11329,#2894);
#2186=LINE('',#11332,#2895);
#2187=LINE('',#11334,#2896);
#2188=LINE('',#11335,#2897);
#2189=LINE('',#11338,#2898);
#2190=LINE('',#11340,#2899);
#2191=LINE('',#11341,#2900);
#2192=LINE('',#11345,#2901);
#2193=LINE('',#11347,#2902);
#2194=LINE('',#11349,#2903);
#2195=LINE('',#11350,#2904);
#2196=LINE('',#11353,#2905);
#2197=LINE('',#11355,#2906);
#2198=LINE('',#11356,#2907);
#2199=LINE('',#11359,#2908);
#2200=LINE('',#11361,#2909);
#2201=LINE('',#11362,#2910);
#2202=LINE('',#11365,#2911);
#2203=LINE('',#11367,#2912);
#2204=LINE('',#11368,#2913);
#2205=LINE('',#11371,#2914);
#2206=LINE('',#11373,#2915);
#2207=LINE('',#11374,#2916);
#2208=LINE('',#11377,#2917);
#2209=LINE('',#11379,#2918);
#2210=LINE('',#11380,#2919);
#2211=LINE('',#11383,#2920);
#2212=LINE('',#11385,#2921);
#2213=LINE('',#11386,#2922);
#2214=LINE('',#11389,#2923);
#2215=LINE('',#11391,#2924);
#2216=LINE('',#11392,#2925);
#2217=LINE('',#11395,#2926);
#2218=LINE('',#11397,#2927);
#2219=LINE('',#11398,#2928);
#2220=LINE('',#11402,#2929);
#2221=LINE('',#11404,#2930);
#2222=LINE('',#11406,#2931);
#2223=LINE('',#11407,#2932);
#2224=LINE('',#11410,#2933);
#2225=LINE('',#11412,#2934);
#2226=LINE('',#11413,#2935);
#2227=LINE('',#11416,#2936);
#2228=LINE('',#11418,#2937);
#2229=LINE('',#11419,#2938);
#2230=LINE('',#11422,#2939);
#2231=LINE('',#11424,#2940);
#2232=LINE('',#11425,#2941);
#2233=LINE('',#11428,#2942);
#2234=LINE('',#11430,#2943);
#2235=LINE('',#11431,#2944);
#2236=LINE('',#11434,#2945);
#2237=LINE('',#11436,#2946);
#2238=LINE('',#11437,#2947);
#2239=LINE('',#11440,#2948);
#2240=LINE('',#11442,#2949);
#2241=LINE('',#11443,#2950);
#2242=LINE('',#11446,#2951);
#2243=LINE('',#11448,#2952);
#2244=LINE('',#11449,#2953);
#2245=LINE('',#11452,#2954);
#2246=LINE('',#11454,#2955);
#2247=LINE('',#11455,#2956);
#2248=LINE('',#11459,#2957);
#2249=LINE('',#11461,#2958);
#2250=LINE('',#11463,#2959);
#2251=LINE('',#11464,#2960);
#2252=LINE('',#11467,#2961);
#2253=LINE('',#11469,#2962);
#2254=LINE('',#11470,#2963);
#2255=LINE('',#11473,#2964);
#2256=LINE('',#11475,#2965);
#2257=LINE('',#11476,#2966);
#2258=LINE('',#11479,#2967);
#2259=LINE('',#11481,#2968);
#2260=LINE('',#11482,#2969);
#2261=LINE('',#11485,#2970);
#2262=LINE('',#11487,#2971);
#2263=LINE('',#11488,#2972);
#2264=LINE('',#11491,#2973);
#2265=LINE('',#11493,#2974);
#2266=LINE('',#11494,#2975);
#2267=LINE('',#11497,#2976);
#2268=LINE('',#11499,#2977);
#2269=LINE('',#11500,#2978);
#2270=LINE('',#11503,#2979);
#2271=LINE('',#11505,#2980);
#2272=LINE('',#11506,#2981);
#2273=LINE('',#11509,#2982);
#2274=LINE('',#11511,#2983);
#2275=LINE('',#11512,#2984);
#2276=LINE('',#11517,#2985);
#2277=LINE('',#11521,#2986);
#2278=LINE('',#11523,#2987);
#2279=LINE('',#11524,#2988);
#2280=LINE('',#11527,#2989);
#2281=LINE('',#11529,#2990);
#2282=LINE('',#11530,#2991);
#2283=LINE('',#11532,#2992);
#2284=LINE('',#11533,#2993);
#2285=LINE('',#11536,#2994);
#2286=LINE('',#11538,#2995);
#2287=LINE('',#11539,#2996);
#2288=LINE('',#11541,#2997);
#2289=LINE('',#11542,#2998);
#2290=LINE('',#11545,#2999);
#2291=LINE('',#11547,#3000);
#2292=LINE('',#11548,#3001);
#2293=LINE('',#11550,#3002);
#2294=LINE('',#11551,#3003);
#2295=LINE('',#11553,#3004);
#2296=LINE('',#11554,#3005);
#2297=LINE('',#11562,#3006);
#2298=LINE('',#11571,#3007);
#2299=LINE('',#11580,#3008);
#2300=LINE('',#11589,#3009);
#2301=LINE('',#11597,#3010);
#2302=LINE('',#11601,#3011);
#2303=LINE('',#11605,#3012);
#2304=LINE('',#11609,#3013);
#2305=LINE('',#11613,#3014);
#2306=LINE('',#11615,#3015);
#2307=LINE('',#11617,#3016);
#2308=LINE('',#11618,#3017);
#2309=LINE('',#11621,#3018);
#2310=LINE('',#11623,#3019);
#2311=LINE('',#11624,#3020);
#2312=LINE('',#11627,#3021);
#2313=LINE('',#11629,#3022);
#2314=LINE('',#11630,#3023);
#2315=LINE('',#11633,#3024);
#2316=LINE('',#11635,#3025);
#2317=LINE('',#11636,#3026);
#2318=LINE('',#11639,#3027);
#2319=LINE('',#11641,#3028);
#2320=LINE('',#11642,#3029);
#2321=LINE('',#11645,#3030);
#2322=LINE('',#11647,#3031);
#2323=LINE('',#11648,#3032);
#2324=LINE('',#11651,#3033);
#2325=LINE('',#11653,#3034);
#2326=LINE('',#11654,#3035);
#2327=LINE('',#11657,#3036);
#2328=LINE('',#11659,#3037);
#2329=LINE('',#11660,#3038);
#2330=LINE('',#11663,#3039);
#2331=LINE('',#11665,#3040);
#2332=LINE('',#11666,#3041);
#2333=LINE('',#11669,#3042);
#2334=LINE('',#11671,#3043);
#2335=LINE('',#11672,#3044);
#2336=LINE('',#11675,#3045);
#2337=LINE('',#11677,#3046);
#2338=LINE('',#11678,#3047);
#2339=LINE('',#11680,#3048);
#2340=LINE('',#11681,#3049);
#2341=LINE('',#11691,#3050);
#2342=LINE('',#11695,#3051);
#2343=LINE('',#11699,#3052);
#2344=LINE('',#11706,#3053);
#2345=LINE('',#11710,#3054);
#2346=LINE('',#11714,#3055);
#2347=LINE('',#11719,#3056);
#2348=LINE('',#11721,#3057);
#2349=LINE('',#11723,#3058);
#2350=LINE('',#11724,#3059);
#2351=LINE('',#11727,#3060);
#2352=LINE('',#11729,#3061);
#2353=LINE('',#11730,#3062);
#2354=LINE('',#11733,#3063);
#2355=LINE('',#11735,#3064);
#2356=LINE('',#11736,#3065);
#2357=LINE('',#11739,#3066);
#2358=LINE('',#11741,#3067);
#2359=LINE('',#11742,#3068);
#2360=LINE('',#11745,#3069);
#2361=LINE('',#11747,#3070);
#2362=LINE('',#11748,#3071);
#2363=LINE('',#11750,#3072);
#2364=LINE('',#11751,#3073);
#2365=LINE('',#11758,#3074);
#2366=LINE('',#11760,#3075);
#2367=LINE('',#11762,#3076);
#2368=LINE('',#11763,#3077);
#2369=LINE('',#11766,#3078);
#2370=LINE('',#11768,#3079);
#2371=LINE('',#11769,#3080);
#2372=LINE('',#11772,#3081);
#2373=LINE('',#11774,#3082);
#2374=LINE('',#11775,#3083);
#2375=LINE('',#11780,#3084);
#2376=LINE('',#11782,#3085);
#2377=LINE('',#11784,#3086);
#2378=LINE('',#11786,#3087);
#2379=LINE('',#11788,#3088);
#2380=LINE('',#11790,#3089);
#2381=LINE('',#11791,#3090);
#2382=LINE('',#11794,#3091);
#2383=LINE('',#11795,#3092);
#2384=LINE('',#11798,#3093);
#2385=LINE('',#11799,#3094);
#2386=LINE('',#11802,#3095);
#2387=LINE('',#11804,#3096);
#2388=LINE('',#11806,#3097);
#2389=LINE('',#11808,#3098);
#2390=LINE('',#11809,#3099);
#2391=LINE('',#11811,#3100);
#2392=LINE('',#11814,#3101);
#2393=LINE('',#11817,#3102);
#2394=LINE('',#11821,#3103);
#2395=LINE('',#11828,#3104);
#2396=LINE('',#11830,#3105);
#2397=LINE('',#11832,#3106);
#2398=LINE('',#11838,#3107);
#2399=LINE('',#11840,#3108);
#2400=LINE('',#11842,#3109);
#2401=LINE('',#11843,#3110);
#2402=LINE('',#11846,#3111);
#2403=LINE('',#11848,#3112);
#2404=LINE('',#11849,#3113);
#2405=LINE('',#11852,#3114);
#2406=LINE('',#11854,#3115);
#2407=LINE('',#11855,#3116);
#2408=LINE('',#11858,#3117);
#2409=LINE('',#11860,#3118);
#2410=LINE('',#11861,#3119);
#2411=LINE('',#11864,#3120);
#2412=LINE('',#11866,#3121);
#2413=LINE('',#11867,#3122);
#2414=LINE('',#11869,#3123);
#2415=LINE('',#11870,#3124);
#2416=LINE('',#11882,#3125);
#2417=LINE('',#11886,#3126);
#2418=LINE('',#11890,#3127);
#2419=LINE('',#11897,#3128);
#2420=LINE('',#11899,#3129);
#2421=LINE('',#11906,#3130);
#2422=LINE('',#11912,#3131);
#2423=LINE('',#11918,#3132);
#2424=LINE('',#11924,#3133);
#2425=LINE('',#11930,#3134);
#2426=LINE('',#11936,#3135);
#2427=LINE('',#11942,#3136);
#2428=LINE('',#11948,#3137);
#2429=LINE('',#11954,#3138);
#2430=LINE('',#11960,#3139);
#2431=LINE('',#11966,#3140);
#2432=LINE('',#11972,#3141);
#2433=LINE('',#11978,#3142);
#2434=LINE('',#11984,#3143);
#2435=LINE('',#11990,#3144);
#2436=LINE('',#11996,#3145);
#2437=LINE('',#12002,#3146);
#2438=LINE('',#12008,#3147);
#2439=LINE('',#12014,#3148);
#2440=LINE('',#12019,#3149);
#2441=LINE('',#12021,#3150);
#2442=LINE('',#12023,#3151);
#2443=LINE('',#12024,#3152);
#2444=LINE('',#12027,#3153);
#2445=LINE('',#12029,#3154);
#2446=LINE('',#12030,#3155);
#2447=LINE('',#12033,#3156);
#2448=LINE('',#12035,#3157);
#2449=LINE('',#12036,#3158);
#2450=LINE('',#12038,#3159);
#2451=LINE('',#12039,#3160);
#2452=LINE('',#12047,#3161);
#2453=LINE('',#12053,#3162);
#2454=LINE('',#12062,#3163);
#2455=LINE('',#12068,#3164);
#2456=LINE('',#12073,#3165);
#2457=LINE('',#12075,#3166);
#2458=LINE('',#12077,#3167);
#2459=LINE('',#12078,#3168);
#2460=LINE('',#12081,#3169);
#2461=LINE('',#12083,#3170);
#2462=LINE('',#12084,#3171);
#2463=LINE('',#12087,#3172);
#2464=LINE('',#12089,#3173);
#2465=LINE('',#12090,#3174);
#2466=LINE('',#12093,#3175);
#2467=LINE('',#12095,#3176);
#2468=LINE('',#12096,#3177);
#2469=LINE('',#12099,#3178);
#2470=LINE('',#12101,#3179);
#2471=LINE('',#12102,#3180);
#2472=LINE('',#12104,#3181);
#2473=LINE('',#12105,#3182);
#2474=LINE('',#12113,#3183);
#2475=LINE('',#12117,#3184);
#2476=LINE('',#12121,#3185);
#2477=LINE('',#12125,#3186);
#2478=LINE('',#12129,#3187);
#2479=LINE('',#12133,#3188);
#2480=LINE('',#12137,#3189);
#2481=LINE('',#12141,#3190);
#2482=LINE('',#12145,#3191);
#2483=LINE('',#12149,#3192);
#2484=LINE('',#12153,#3193);
#2485=LINE('',#12157,#3194);
#2486=LINE('',#12161,#3195);
#2487=LINE('',#12165,#3196);
#2488=LINE('',#12169,#3197);
#2489=LINE('',#12173,#3198);
#2490=LINE('',#12175,#3199);
#2491=LINE('',#12177,#3200);
#2492=LINE('',#12179,#3201);
#2493=LINE('',#12181,#3202);
#2494=LINE('',#12183,#3203);
#2495=LINE('',#12184,#3204);
#2496=LINE('',#12186,#3205);
#2497=LINE('',#12188,#3206);
#2498=LINE('',#12190,#3207);
#2499=LINE('',#12192,#3208);
#2500=LINE('',#12194,#3209);
#2501=LINE('',#12195,#3210);
#2502=LINE('',#12198,#3211);
#2503=LINE('',#12200,#3212);
#2504=LINE('',#12202,#3213);
#2505=LINE('',#12204,#3214);
#2506=LINE('',#12205,#3215);
#2507=LINE('',#12207,#3216);
#2508=LINE('',#12209,#3217);
#2509=LINE('',#12211,#3218);
#2510=LINE('',#12213,#3219);
#2511=LINE('',#12214,#3220);
#2512=LINE('',#12217,#3221);
#2513=LINE('',#12218,#3222);
#2514=LINE('',#12221,#3223);
#2515=LINE('',#12222,#3224);
#2516=LINE('',#12225,#3225);
#2517=LINE('',#12226,#3226);
#2518=LINE('',#12229,#3227);
#2519=LINE('',#12230,#3228);
#2520=LINE('',#12232,#3229);
#2521=LINE('',#12235,#3230);
#2522=LINE('',#12236,#3231);
#2523=LINE('',#12239,#3232);
#2524=LINE('',#12240,#3233);
#2525=LINE('',#12243,#3234);
#2526=LINE('',#12244,#3235);
#2527=LINE('',#12247,#3236);
#2528=LINE('',#12248,#3237);
#2529=LINE('',#12250,#3238);
#2530=LINE('',#12256,#3239);
#2531=LINE('',#12258,#3240);
#2532=LINE('',#12260,#3241);
#2533=LINE('',#12261,#3242);
#2534=LINE('',#12264,#3243);
#2535=LINE('',#12266,#3244);
#2536=LINE('',#12267,#3245);
#2537=LINE('',#12270,#3246);
#2538=LINE('',#12272,#3247);
#2539=LINE('',#12273,#3248);
#2540=LINE('',#12276,#3249);
#2541=LINE('',#12278,#3250);
#2542=LINE('',#12279,#3251);
#2543=LINE('',#12282,#3252);
#2544=LINE('',#12284,#3253);
#2545=LINE('',#12285,#3254);
#2546=LINE('',#12288,#3255);
#2547=LINE('',#12290,#3256);
#2548=LINE('',#12291,#3257);
#2549=LINE('',#12294,#3258);
#2550=LINE('',#12296,#3259);
#2551=LINE('',#12297,#3260);
#2552=LINE('',#12299,#3261);
#2553=LINE('',#12300,#3262);
#2554=LINE('',#12307,#3263);
#2555=LINE('',#12309,#3264);
#2556=LINE('',#12311,#3265);
#2557=LINE('',#12312,#3266);
#2558=LINE('',#12315,#3267);
#2559=LINE('',#12317,#3268);
#2560=LINE('',#12318,#3269);
#2561=LINE('',#12321,#3270);
#2562=LINE('',#12323,#3271);
#2563=LINE('',#12324,#3272);
#2564=LINE('',#12327,#3273);
#2565=LINE('',#12329,#3274);
#2566=LINE('',#12330,#3275);
#2567=LINE('',#12333,#3276);
#2568=LINE('',#12335,#3277);
#2569=LINE('',#12336,#3278);
#2570=LINE('',#12339,#3279);
#2571=LINE('',#12341,#3280);
#2572=LINE('',#12342,#3281);
#2573=LINE('',#12345,#3282);
#2574=LINE('',#12347,#3283);
#2575=LINE('',#12348,#3284);
#2576=LINE('',#12350,#3285);
#2577=LINE('',#12351,#3286);
#2578=LINE('',#12362,#3287);
#2579=LINE('',#12366,#3288);
#2580=LINE('',#12373,#3289);
#2581=LINE('',#12453,#3290);
#2582=LINE('',#12457,#3291);
#2583=LINE('',#12461,#3292);
#2584=LINE('',#12468,#3293);
#2585=LINE('',#12472,#3294);
#2586=LINE('',#12476,#3295);
#2587=LINE('',#12481,#3296);
#2588=LINE('',#12483,#3297);
#2589=LINE('',#12485,#3298);
#2590=LINE('',#12486,#3299);
#2591=LINE('',#12489,#3300);
#2592=LINE('',#12491,#3301);
#2593=LINE('',#12492,#3302);
#2594=LINE('',#12495,#3303);
#2595=LINE('',#12497,#3304);
#2596=LINE('',#12498,#3305);
#2597=LINE('',#12501,#3306);
#2598=LINE('',#12503,#3307);
#2599=LINE('',#12504,#3308);
#2600=LINE('',#12507,#3309);
#2601=LINE('',#12509,#3310);
#2602=LINE('',#12510,#3311);
#2603=LINE('',#12512,#3312);
#2604=LINE('',#12513,#3313);
#2605=LINE('',#12521,#3314);
#2606=LINE('',#12527,#3315);
#2607=LINE('',#12538,#3316);
#2608=LINE('',#12542,#3317);
#2609=LINE('',#12546,#3318);
#2610=LINE('',#12553,#3319);
#2611=LINE('',#12557,#3320);
#2612=LINE('',#12561,#3321);
#2613=LINE('',#12566,#3322);
#2614=LINE('',#12568,#3323);
#2615=LINE('',#12570,#3324);
#2616=LINE('',#12571,#3325);
#2617=LINE('',#12574,#3326);
#2618=LINE('',#12576,#3327);
#2619=LINE('',#12577,#3328);
#2620=LINE('',#12580,#3329);
#2621=LINE('',#12582,#3330);
#2622=LINE('',#12583,#3331);
#2623=LINE('',#12586,#3332);
#2624=LINE('',#12588,#3333);
#2625=LINE('',#12589,#3334);
#2626=LINE('',#12592,#3335);
#2627=LINE('',#12594,#3336);
#2628=LINE('',#12595,#3337);
#2629=LINE('',#12597,#3338);
#2630=LINE('',#12598,#3339);
#2631=LINE('',#12606,#3340);
#2632=LINE('',#12610,#3341);
#2633=LINE('',#12617,#3342);
#2634=LINE('',#12624,#3343);
#2635=LINE('',#12626,#3344);
#2636=LINE('',#12628,#3345);
#2637=LINE('',#12629,#3346);
#2638=LINE('',#12632,#3347);
#2639=LINE('',#12634,#3348);
#2640=LINE('',#12635,#3349);
#2641=LINE('',#12638,#3350);
#2642=LINE('',#12640,#3351);
#2643=LINE('',#12641,#3352);
#2644=LINE('',#12644,#3353);
#2645=LINE('',#12646,#3354);
#2646=LINE('',#12647,#3355);
#2647=LINE('',#12650,#3356);
#2648=LINE('',#12652,#3357);
#2649=LINE('',#12653,#3358);
#2650=LINE('',#12655,#3359);
#2651=LINE('',#12656,#3360);
#2652=LINE('',#12668,#3361);
#2653=LINE('',#12672,#3362);
#2654=LINE('',#12676,#3363);
#2655=LINE('',#12683,#3364);
#2656=LINE('',#12685,#3365);
#2657=VECTOR('',#8497,0.164999999999999);
#2658=VECTOR('',#8504,0.164999999999999);
#2659=VECTOR('',#8511,0.164999999999999);
#2660=VECTOR('',#8518,0.164999999999999);
#2661=VECTOR('',#8525,0.275);
#2662=VECTOR('',#8532,0.274999999999999);
#2663=VECTOR('',#8537,1.);
#2664=VECTOR('',#8538,1.);
#2665=VECTOR('',#8539,1.);
#2666=VECTOR('',#8540,1.);
#2667=VECTOR('',#8543,1.);
#2668=VECTOR('',#8544,1.);
#2669=VECTOR('',#8545,1.);
#2670=VECTOR('',#8548,1.);
#2671=VECTOR('',#8549,1.);
#2672=VECTOR('',#8550,1.);
#2673=VECTOR('',#8553,1.);
#2674=VECTOR('',#8554,1.);
#2675=VECTOR('',#8565,0.164999999999999);
#2676=VECTOR('',#8572,0.164999999999999);
#2677=VECTOR('',#8579,0.164999999999999);
#2678=VECTOR('',#8586,0.164999999999999);
#2679=VECTOR('',#8593,0.275);
#2680=VECTOR('',#8600,0.274999999999999);
#2681=VECTOR('',#8605,1.);
#2682=VECTOR('',#8606,1.);
#2683=VECTOR('',#8607,1.);
#2684=VECTOR('',#8608,1.);
#2685=VECTOR('',#8611,1.);
#2686=VECTOR('',#8612,1.);
#2687=VECTOR('',#8613,1.);
#2688=VECTOR('',#8616,1.);
#2689=VECTOR('',#8617,1.);
#2690=VECTOR('',#8618,1.);
#2691=VECTOR('',#8621,1.);
#2692=VECTOR('',#8622,1.);
#2693=VECTOR('',#8633,0.275);
#2694=VECTOR('',#8640,0.275);
#2695=VECTOR('',#8645,1.);
#2696=VECTOR('',#8646,1.);
#2697=VECTOR('',#8647,1.);
#2698=VECTOR('',#8648,1.);
#2699=VECTOR('',#8651,1.);
#2700=VECTOR('',#8652,1.);
#2701=VECTOR('',#8653,1.);
#2702=VECTOR('',#8656,1.);
#2703=VECTOR('',#8657,1.);
#2704=VECTOR('',#8658,1.);
#2705=VECTOR('',#8661,1.);
#2706=VECTOR('',#8662,1.);
#2707=VECTOR('',#8673,0.275);
#2708=VECTOR('',#8680,0.275);
#2709=VECTOR('',#8685,1.);
#2710=VECTOR('',#8686,1.);
#2711=VECTOR('',#8687,1.);
#2712=VECTOR('',#8688,1.);
#2713=VECTOR('',#8691,1.);
#2714=VECTOR('',#8692,1.);
#2715=VECTOR('',#8693,1.);
#2716=VECTOR('',#8696,1.);
#2717=VECTOR('',#8697,1.);
#2718=VECTOR('',#8698,1.);
#2719=VECTOR('',#8701,1.);
#2720=VECTOR('',#8702,1.);
#2721=VECTOR('',#8711,1.);
#2722=VECTOR('',#8712,1.);
#2723=VECTOR('',#8713,1.);
#2724=VECTOR('',#8714,1.);
#2725=VECTOR('',#8717,1.);
#2726=VECTOR('',#8718,1.);
#2727=VECTOR('',#8719,1.);
#2728=VECTOR('',#8722,1.);
#2729=VECTOR('',#8723,1.);
#2730=VECTOR('',#8724,1.);
#2731=VECTOR('',#8727,1.);
#2732=VECTOR('',#8728,1.);
#2733=VECTOR('',#8737,1.);
#2734=VECTOR('',#8738,1.);
#2735=VECTOR('',#8739,1.);
#2736=VECTOR('',#8740,1.);
#2737=VECTOR('',#8743,1.);
#2738=VECTOR('',#8744,1.);
#2739=VECTOR('',#8745,1.);
#2740=VECTOR('',#8748,1.);
#2741=VECTOR('',#8749,1.);
#2742=VECTOR('',#8750,1.);
#2743=VECTOR('',#8753,1.);
#2744=VECTOR('',#8754,1.);
#2745=VECTOR('',#8765,0.274999999999999);
#2746=VECTOR('',#8772,0.274999999999999);
#2747=VECTOR('',#8777,1.);
#2748=VECTOR('',#8778,1.);
#2749=VECTOR('',#8779,1.);
#2750=VECTOR('',#8780,1.);
#2751=VECTOR('',#8783,1.);
#2752=VECTOR('',#8784,1.);
#2753=VECTOR('',#8785,1.);
#2754=VECTOR('',#8788,1.);
#2755=VECTOR('',#8789,1.);
#2756=VECTOR('',#8790,1.);
#2757=VECTOR('',#8793,1.);
#2758=VECTOR('',#8794,1.);
#2759=VECTOR('',#8805,0.274999999999999);
#2760=VECTOR('',#8812,0.274999999999999);
#2761=VECTOR('',#8817,1.);
#2762=VECTOR('',#8818,1.);
#2763=VECTOR('',#8819,1.);
#2764=VECTOR('',#8820,1.);
#2765=VECTOR('',#8823,1.);
#2766=VECTOR('',#8824,1.);
#2767=VECTOR('',#8825,1.);
#2768=VECTOR('',#8828,1.);
#2769=VECTOR('',#8829,1.);
#2770=VECTOR('',#8830,1.);
#2771=VECTOR('',#8833,1.);
#2772=VECTOR('',#8834,1.);
#2773=VECTOR('',#8843,1.);
#2774=VECTOR('',#8844,1.);
#2775=VECTOR('',#8845,1.);
#2776=VECTOR('',#8846,1.);
#2777=VECTOR('',#8849,1.);
#2778=VECTOR('',#8850,1.);
#2779=VECTOR('',#8851,1.);
#2780=VECTOR('',#8854,1.);
#2781=VECTOR('',#8855,1.);
#2782=VECTOR('',#8856,1.);
#2783=VECTOR('',#8859,1.);
#2784=VECTOR('',#8860,1.);
#2785=VECTOR('',#8869,1.);
#2786=VECTOR('',#8870,1.);
#2787=VECTOR('',#8871,1.);
#2788=VECTOR('',#8872,1.);
#2789=VECTOR('',#8875,1.);
#2790=VECTOR('',#8876,1.);
#2791=VECTOR('',#8877,1.);
#2792=VECTOR('',#8880,1.);
#2793=VECTOR('',#8881,1.);
#2794=VECTOR('',#8882,1.);
#2795=VECTOR('',#8885,1.);
#2796=VECTOR('',#8886,1.);
#2797=VECTOR('',#8895,1.);
#2798=VECTOR('',#8898,1.);
#2799=VECTOR('',#8903,1.);
#2800=VECTOR('',#8906,1.);
#2801=VECTOR('',#8915,1.);
#2802=VECTOR('',#8918,1.);
#2803=VECTOR('',#8923,1.);
#2804=VECTOR('',#8926,1.);
#2805=VECTOR('',#8935,1.);
#2806=VECTOR('',#8936,1.);
#2807=VECTOR('',#8937,1.);
#2808=VECTOR('',#8940,1.);
#2809=VECTOR('',#8941,1.);
#2810=VECTOR('',#8944,1.);
#2811=VECTOR('',#8945,1.);
#2812=VECTOR('',#8946,1.);
#2813=VECTOR('',#8951,0.275);
#2814=VECTOR('',#8956,0.275);
#2815=VECTOR('',#8959,1.);
#2816=VECTOR('',#8960,1.);
#2817=VECTOR('',#8961,1.);
#2818=VECTOR('',#8964,1.);
#2819=VECTOR('',#8965,1.);
#2820=VECTOR('',#8968,1.);
#2821=VECTOR('',#8969,1.);
#2822=VECTOR('',#8972,1.);
#2823=VECTOR('',#8979,1.);
#2824=VECTOR('',#8980,1.);
#2825=VECTOR('',#8981,1.);
#2826=VECTOR('',#8982,1.);
#2827=VECTOR('',#8985,1.);
#2828=VECTOR('',#8986,1.);
#2829=VECTOR('',#8987,1.);
#2830=VECTOR('',#8990,1.);
#2831=VECTOR('',#8991,1.);
#2832=VECTOR('',#8992,1.);
#2833=VECTOR('',#8995,1.);
#2834=VECTOR('',#8996,1.);
#2835=VECTOR('',#9005,1.);
#2836=VECTOR('',#9008,1.);
#2837=VECTOR('',#9013,1.);
#2838=VECTOR('',#9016,1.);
#2839=VECTOR('',#9025,1.);
#2840=VECTOR('',#9028,1.);
#2841=VECTOR('',#9033,1.);
#2842=VECTOR('',#9036,1.);
#2843=VECTOR('',#9045,1.);
#2844=VECTOR('',#9046,1.);
#2845=VECTOR('',#9047,1.);
#2846=VECTOR('',#9050,1.);
#2847=VECTOR('',#9051,1.);
#2848=VECTOR('',#9054,1.);
#2849=VECTOR('',#9055,1.);
#2850=VECTOR('',#9056,1.);
#2851=VECTOR('',#9061,0.274999999999999);
#2852=VECTOR('',#9066,0.274999999999999);
#2853=VECTOR('',#9069,1.);
#2854=VECTOR('',#9070,1.);
#2855=VECTOR('',#9071,1.);
#2856=VECTOR('',#9074,1.);
#2857=VECTOR('',#9075,1.);
#2858=VECTOR('',#9078,1.);
#2859=VECTOR('',#9079,1.);
#2860=VECTOR('',#9082,1.);
#2861=VECTOR('',#9089,1.);
#2862=VECTOR('',#9090,1.);
#2863=VECTOR('',#9091,1.);
#2864=VECTOR('',#9092,1.);
#2865=VECTOR('',#9095,1.);
#2866=VECTOR('',#9096,1.);
#2867=VECTOR('',#9097,1.);
#2868=VECTOR('',#9100,1.);
#2869=VECTOR('',#9101,1.);
#2870=VECTOR('',#9102,1.);
#2871=VECTOR('',#9105,1.);
#2872=VECTOR('',#9106,1.);
#2873=VECTOR('',#9115,1.);
#2874=VECTOR('',#9116,1.);
#2875=VECTOR('',#9117,1.);
#2876=VECTOR('',#9118,1.);
#2877=VECTOR('',#9121,1.);
#2878=VECTOR('',#9122,1.);
#2879=VECTOR('',#9123,1.);
#2880=VECTOR('',#9126,1.);
#2881=VECTOR('',#9127,1.);
#2882=VECTOR('',#9128,1.);
#2883=VECTOR('',#9131,1.);
#2884=VECTOR('',#9132,1.);
#2885=VECTOR('',#9133,1.);
#2886=VECTOR('',#9136,1.);
#2887=VECTOR('',#9137,1.);
#2888=VECTOR('',#9138,1.);
#2889=VECTOR('',#9141,1.);
#2890=VECTOR('',#9142,1.);
#2891=VECTOR('',#9143,1.);
#2892=VECTOR('',#9146,1.);
#2893=VECTOR('',#9147,1.);
#2894=VECTOR('',#9148,1.);
#2895=VECTOR('',#9151,1.);
#2896=VECTOR('',#9152,1.);
#2897=VECTOR('',#9153,1.);
#2898=VECTOR('',#9156,1.);
#2899=VECTOR('',#9157,1.);
#2900=VECTOR('',#9158,1.);
#2901=VECTOR('',#9161,1.);
#2902=VECTOR('',#9162,1.);
#2903=VECTOR('',#9163,1.);
#2904=VECTOR('',#9164,1.);
#2905=VECTOR('',#9167,1.);
#2906=VECTOR('',#9168,1.);
#2907=VECTOR('',#9169,1.);
#2908=VECTOR('',#9172,1.);
#2909=VECTOR('',#9173,1.);
#2910=VECTOR('',#9174,1.);
#2911=VECTOR('',#9177,1.);
#2912=VECTOR('',#9178,1.);
#2913=VECTOR('',#9179,1.);
#2914=VECTOR('',#9182,1.);
#2915=VECTOR('',#9183,1.);
#2916=VECTOR('',#9184,1.);
#2917=VECTOR('',#9187,1.);
#2918=VECTOR('',#9188,1.);
#2919=VECTOR('',#9189,1.);
#2920=VECTOR('',#9192,1.);
#2921=VECTOR('',#9193,1.);
#2922=VECTOR('',#9194,1.);
#2923=VECTOR('',#9197,1.);
#2924=VECTOR('',#9198,1.);
#2925=VECTOR('',#9199,1.);
#2926=VECTOR('',#9202,1.);
#2927=VECTOR('',#9203,1.);
#2928=VECTOR('',#9204,1.);
#2929=VECTOR('',#9207,1.);
#2930=VECTOR('',#9208,1.);
#2931=VECTOR('',#9209,1.);
#2932=VECTOR('',#9210,1.);
#2933=VECTOR('',#9213,1.);
#2934=VECTOR('',#9214,1.);
#2935=VECTOR('',#9215,1.);
#2936=VECTOR('',#9218,1.);
#2937=VECTOR('',#9219,1.);
#2938=VECTOR('',#9220,1.);
#2939=VECTOR('',#9223,1.);
#2940=VECTOR('',#9224,1.);
#2941=VECTOR('',#9225,1.);
#2942=VECTOR('',#9228,1.);
#2943=VECTOR('',#9229,1.);
#2944=VECTOR('',#9230,1.);
#2945=VECTOR('',#9233,1.);
#2946=VECTOR('',#9234,1.);
#2947=VECTOR('',#9235,1.);
#2948=VECTOR('',#9238,1.);
#2949=VECTOR('',#9239,1.);
#2950=VECTOR('',#9240,1.);
#2951=VECTOR('',#9243,1.);
#2952=VECTOR('',#9244,1.);
#2953=VECTOR('',#9245,1.);
#2954=VECTOR('',#9248,1.);
#2955=VECTOR('',#9249,1.);
#2956=VECTOR('',#9250,1.);
#2957=VECTOR('',#9253,1.);
#2958=VECTOR('',#9254,1.);
#2959=VECTOR('',#9255,1.);
#2960=VECTOR('',#9256,1.);
#2961=VECTOR('',#9259,1.);
#2962=VECTOR('',#9260,1.);
#2963=VECTOR('',#9261,1.);
#2964=VECTOR('',#9264,1.);
#2965=VECTOR('',#9265,1.);
#2966=VECTOR('',#9266,1.);
#2967=VECTOR('',#9269,1.);
#2968=VECTOR('',#9270,1.);
#2969=VECTOR('',#9271,1.);
#2970=VECTOR('',#9274,1.);
#2971=VECTOR('',#9275,1.);
#2972=VECTOR('',#9276,1.);
#2973=VECTOR('',#9279,1.);
#2974=VECTOR('',#9280,1.);
#2975=VECTOR('',#9281,1.);
#2976=VECTOR('',#9284,1.);
#2977=VECTOR('',#9285,1.);
#2978=VECTOR('',#9286,1.);
#2979=VECTOR('',#9289,1.);
#2980=VECTOR('',#9290,1.);
#2981=VECTOR('',#9291,1.);
#2982=VECTOR('',#9294,1.);
#2983=VECTOR('',#9295,1.);
#2984=VECTOR('',#9296,1.);
#2985=VECTOR('',#9301,0.21);
#2986=VECTOR('',#9306,1.);
#2987=VECTOR('',#9307,1.);
#2988=VECTOR('',#9308,1.);
#2989=VECTOR('',#9311,1.);
#2990=VECTOR('',#9312,1.);
#2991=VECTOR('',#9313,1.);
#2992=VECTOR('',#9316,1.);
#2993=VECTOR('',#9317,1.);
#2994=VECTOR('',#9320,1.);
#2995=VECTOR('',#9321,1.);
#2996=VECTOR('',#9322,1.);
#2997=VECTOR('',#9325,1.);
#2998=VECTOR('',#9326,1.);
#2999=VECTOR('',#9329,1.);
#3000=VECTOR('',#9330,1.);
#3001=VECTOR('',#9331,1.);
#3002=VECTOR('',#9334,1.);
#3003=VECTOR('',#9335,1.);
#3004=VECTOR('',#9338,1.);
#3005=VECTOR('',#9339,1.);
#3006=VECTOR('',#9350,0.375);
#3007=VECTOR('',#9361,0.375);
#3008=VECTOR('',#9372,0.375);
#3009=VECTOR('',#9383,0.375);
#3010=VECTOR('',#9394,0.225);
#3011=VECTOR('',#9399,0.225);
#3012=VECTOR('',#9404,0.225);
#3013=VECTOR('',#9409,0.225000000000001);
#3014=VECTOR('',#9412,1.);
#3015=VECTOR('',#9413,1.);
#3016=VECTOR('',#9414,1.);
#3017=VECTOR('',#9415,1.);
#3018=VECTOR('',#9418,1.);
#3019=VECTOR('',#9419,1.);
#3020=VECTOR('',#9420,1.);
#3021=VECTOR('',#9423,1.);
#3022=VECTOR('',#9424,1.);
#3023=VECTOR('',#9425,1.);
#3024=VECTOR('',#9428,1.);
#3025=VECTOR('',#9429,1.);
#3026=VECTOR('',#9430,1.);
#3027=VECTOR('',#9433,1.);
#3028=VECTOR('',#9434,1.);
#3029=VECTOR('',#9435,1.);
#3030=VECTOR('',#9438,1.);
#3031=VECTOR('',#9439,1.);
#3032=VECTOR('',#9440,1.);
#3033=VECTOR('',#9443,1.);
#3034=VECTOR('',#9444,1.);
#3035=VECTOR('',#9445,1.);
#3036=VECTOR('',#9448,1.);
#3037=VECTOR('',#9449,1.);
#3038=VECTOR('',#9450,1.);
#3039=VECTOR('',#9453,1.);
#3040=VECTOR('',#9454,1.);
#3041=VECTOR('',#9455,1.);
#3042=VECTOR('',#9458,1.);
#3043=VECTOR('',#9459,1.);
#3044=VECTOR('',#9460,1.);
#3045=VECTOR('',#9463,1.);
#3046=VECTOR('',#9464,1.);
#3047=VECTOR('',#9465,1.);
#3048=VECTOR('',#9468,1.);
#3049=VECTOR('',#9469,1.);
#3050=VECTOR('',#9484,0.325);
#3051=VECTOR('',#9489,0.35);
#3052=VECTOR('',#9494,0.335);
#3053=VECTOR('',#9503,0.21);
#3054=VECTOR('',#9508,0.2);
#3055=VECTOR('',#9513,0.18);
#3056=VECTOR('',#9518,1.);
#3057=VECTOR('',#9519,1.);
#3058=VECTOR('',#9520,1.);
#3059=VECTOR('',#9521,1.);
#3060=VECTOR('',#9524,1.);
#3061=VECTOR('',#9525,1.);
#3062=VECTOR('',#9526,1.);
#3063=VECTOR('',#9529,1.);
#3064=VECTOR('',#9530,1.);
#3065=VECTOR('',#9531,1.);
#3066=VECTOR('',#9534,1.);
#3067=VECTOR('',#9535,1.);
#3068=VECTOR('',#9536,1.);
#3069=VECTOR('',#9539,1.);
#3070=VECTOR('',#9540,1.);
#3071=VECTOR('',#9541,1.);
#3072=VECTOR('',#9544,1.);
#3073=VECTOR('',#9545,1.);
#3074=VECTOR('',#9554,1.);
#3075=VECTOR('',#9555,1.);
#3076=VECTOR('',#9556,1.);
#3077=VECTOR('',#9557,1.);
#3078=VECTOR('',#9560,1.);
#3079=VECTOR('',#9561,1.);
#3080=VECTOR('',#9562,1.);
#3081=VECTOR('',#9565,1.);
#3082=VECTOR('',#9566,1.);
#3083=VECTOR('',#9567,1.);
#3084=VECTOR('',#9572,1.);
#3085=VECTOR('',#9573,1.);
#3086=VECTOR('',#9574,1.);
#3087=VECTOR('',#9575,1.);
#3088=VECTOR('',#9576,1.);
#3089=VECTOR('',#9577,1.);
#3090=VECTOR('',#9578,1.);
#3091=VECTOR('',#9581,1.);
#3092=VECTOR('',#9582,1.);
#3093=VECTOR('',#9585,1.);
#3094=VECTOR('',#9586,1.);
#3095=VECTOR('',#9589,1.);
#3096=VECTOR('',#9590,1.);
#3097=VECTOR('',#9591,1.);
#3098=VECTOR('',#9592,1.);
#3099=VECTOR('',#9593,1.);
#3100=VECTOR('',#9596,1.);
#3101=VECTOR('',#9599,1.);
#3102=VECTOR('',#9602,1.);
#3103=VECTOR('',#9607,0.21);
#3104=VECTOR('',#9616,1.);
#3105=VECTOR('',#9619,1.);
#3106=VECTOR('',#9622,1.);
#3107=VECTOR('',#9629,1.);
#3108=VECTOR('',#9630,1.);
#3109=VECTOR('',#9631,1.);
#3110=VECTOR('',#9632,1.);
#3111=VECTOR('',#9635,1.);
#3112=VECTOR('',#9636,1.);
#3113=VECTOR('',#9637,1.);
#3114=VECTOR('',#9640,1.);
#3115=VECTOR('',#9641,1.);
#3116=VECTOR('',#9642,1.);
#3117=VECTOR('',#9645,1.);
#3118=VECTOR('',#9646,1.);
#3119=VECTOR('',#9647,1.);
#3120=VECTOR('',#9650,1.);
#3121=VECTOR('',#9651,1.);
#3122=VECTOR('',#9652,1.);
#3123=VECTOR('',#9655,1.);
#3124=VECTOR('',#9656,1.);
#3125=VECTOR('',#9673,0.4);
#3126=VECTOR('',#9678,0.425);
#3127=VECTOR('',#9683,0.41);
#3128=VECTOR('',#9692,0.26);
#3129=VECTOR('',#9695,0.25);
#3130=VECTOR('',#9704,0.164999999999999);
#3131=VECTOR('',#9711,0.164999999999999);
#3132=VECTOR('',#9718,0.25);
#3133=VECTOR('',#9725,0.274999999999999);
#3134=VECTOR('',#9732,0.274999999999999);
#3135=VECTOR('',#9739,0.274999999999999);
#3136=VECTOR('',#9746,0.274999999999999);
#3137=VECTOR('',#9753,0.274999999999999);
#3138=VECTOR('',#9760,0.275);
#3139=VECTOR('',#9767,0.275);
#3140=VECTOR('',#9774,0.274999999999999);
#3141=VECTOR('',#9781,0.274999999999999);
#3142=VECTOR('',#9788,0.274999999999999);
#3143=VECTOR('',#9795,0.274999999999999);
#3144=VECTOR('',#9802,0.274999999999999);
#3145=VECTOR('',#9809,0.274999999999999);
#3146=VECTOR('',#9816,0.275);
#3147=VECTOR('',#9823,0.275);
#3148=VECTOR('',#9830,0.274999999999999);
#3149=VECTOR('',#9835,1.);
#3150=VECTOR('',#9836,1.);
#3151=VECTOR('',#9837,1.);
#3152=VECTOR('',#9838,1.);
#3153=VECTOR('',#9841,1.);
#3154=VECTOR('',#9842,1.);
#3155=VECTOR('',#9843,1.);
#3156=VECTOR('',#9846,1.);
#3157=VECTOR('',#9847,1.);
#3158=VECTOR('',#9848,1.);
#3159=VECTOR('',#9851,1.);
#3160=VECTOR('',#9852,1.);
#3161=VECTOR('',#9863,0.329999999999998);
#3162=VECTOR('',#9870,1.5);
#3163=VECTOR('',#9883,0.225000000000001);
#3164=VECTOR('',#9890,0.225000000000001);
#3165=VECTOR('',#9895,1.);
#3166=VECTOR('',#9896,1.);
#3167=VECTOR('',#9897,1.);
#3168=VECTOR('',#9898,1.);
#3169=VECTOR('',#9901,1.);
#3170=VECTOR('',#9902,1.);
#3171=VECTOR('',#9903,1.);
#3172=VECTOR('',#9906,1.);
#3173=VECTOR('',#9907,1.);
#3174=VECTOR('',#9908,1.);
#3175=VECTOR('',#9911,1.);
#3176=VECTOR('',#9912,1.);
#3177=VECTOR('',#9913,1.);
#3178=VECTOR('',#9916,1.);
#3179=VECTOR('',#9917,1.);
#3180=VECTOR('',#9918,1.);
#3181=VECTOR('',#9921,1.);
#3182=VECTOR('',#9922,1.);
#3183=VECTOR('',#9933,1.);
#3184=VECTOR('',#9938,1.);
#3185=VECTOR('',#9941,0.21);
#3186=VECTOR('',#9946,1.);
#3187=VECTOR('',#9949,1.);
#3188=VECTOR('',#9954,1.);
#3189=VECTOR('',#9957,0.21);
#3190=VECTOR('',#9962,1.);
#3191=VECTOR('',#9965,1.);
#3192=VECTOR('',#9970,1.);
#3193=VECTOR('',#9973,0.21);
#3194=VECTOR('',#9978,1.);
#3195=VECTOR('',#9981,1.);
#3196=VECTOR('',#9986,1.);
#3197=VECTOR('',#9989,0.21);
#3198=VECTOR('',#9994,1.);
#3199=VECTOR('',#9997,1.);
#3200=VECTOR('',#9998,1.);
#3201=VECTOR('',#9999,1.);
#3202=VECTOR('',#10000,1.);
#3203=VECTOR('',#10001,1.);
#3204=VECTOR('',#10002,1.);
#3205=VECTOR('',#10005,1.);
#3206=VECTOR('',#10006,1.);
#3207=VECTOR('',#10007,1.);
#3208=VECTOR('',#10008,1.);
#3209=VECTOR('',#10009,1.);
#3210=VECTOR('',#10010,1.);
#3211=VECTOR('',#10013,1.);
#3212=VECTOR('',#10014,1.);
#3213=VECTOR('',#10015,1.);
#3214=VECTOR('',#10016,1.);
#3215=VECTOR('',#10017,1.);
#3216=VECTOR('',#10018,1.);
#3217=VECTOR('',#10019,1.);
#3218=VECTOR('',#10020,1.);
#3219=VECTOR('',#10021,1.);
#3220=VECTOR('',#10022,1.);
#3221=VECTOR('',#10025,1.);
#3222=VECTOR('',#10026,1.);
#3223=VECTOR('',#10029,1.);
#3224=VECTOR('',#10030,1.);
#3225=VECTOR('',#10033,1.);
#3226=VECTOR('',#10034,1.);
#3227=VECTOR('',#10037,1.);
#3228=VECTOR('',#10038,1.);
#3229=VECTOR('',#10041,1.);
#3230=VECTOR('',#10044,1.);
#3231=VECTOR('',#10045,1.);
#3232=VECTOR('',#10048,1.);
#3233=VECTOR('',#10049,1.);
#3234=VECTOR('',#10052,1.);
#3235=VECTOR('',#10053,1.);
#3236=VECTOR('',#10056,1.);
#3237=VECTOR('',#10057,1.);
#3238=VECTOR('',#10060,1.);
#3239=VECTOR('',#10067,1.);
#3240=VECTOR('',#10068,1.);
#3241=VECTOR('',#10069,1.);
#3242=VECTOR('',#10070,1.);
#3243=VECTOR('',#10073,1.);
#3244=VECTOR('',#10074,1.);
#3245=VECTOR('',#10075,1.);
#3246=VECTOR('',#10078,1.);
#3247=VECTOR('',#10079,1.);
#3248=VECTOR('',#10080,1.);
#3249=VECTOR('',#10083,1.);
#3250=VECTOR('',#10084,1.);
#3251=VECTOR('',#10085,1.);
#3252=VECTOR('',#10088,1.);
#3253=VECTOR('',#10089,1.);
#3254=VECTOR('',#10090,1.);
#3255=VECTOR('',#10093,1.);
#3256=VECTOR('',#10094,1.);
#3257=VECTOR('',#10095,1.);
#3258=VECTOR('',#10098,1.);
#3259=VECTOR('',#10099,1.);
#3260=VECTOR('',#10100,1.);
#3261=VECTOR('',#10103,1.);
#3262=VECTOR('',#10104,1.);
#3263=VECTOR('',#10113,1.);
#3264=VECTOR('',#10114,1.);
#3265=VECTOR('',#10115,1.);
#3266=VECTOR('',#10116,1.);
#3267=VECTOR('',#10119,1.);
#3268=VECTOR('',#10120,1.);
#3269=VECTOR('',#10121,1.);
#3270=VECTOR('',#10124,1.);
#3271=VECTOR('',#10125,1.);
#3272=VECTOR('',#10126,1.);
#3273=VECTOR('',#10129,1.);
#3274=VECTOR('',#10130,1.);
#3275=VECTOR('',#10131,1.);
#3276=VECTOR('',#10134,1.);
#3277=VECTOR('',#10135,1.);
#3278=VECTOR('',#10136,1.);
#3279=VECTOR('',#10139,1.);
#3280=VECTOR('',#10140,1.);
#3281=VECTOR('',#10141,1.);
#3282=VECTOR('',#10144,1.);
#3283=VECTOR('',#10145,1.);
#3284=VECTOR('',#10146,1.);
#3285=VECTOR('',#10149,1.);
#3286=VECTOR('',#10150,1.);
#3287=VECTOR('',#10167,0.275);
#3288=VECTOR('',#10172,0.265);
#3289=VECTOR('',#10181,0.5);
#3290=VECTOR('',#10336,0.4);
#3291=VECTOR('',#10341,0.425);
#3292=VECTOR('',#10346,0.41);
#3293=VECTOR('',#10355,0.26);
#3294=VECTOR('',#10360,0.25);
#3295=VECTOR('',#10365,0.225);
#3296=VECTOR('',#10370,1.);
#3297=VECTOR('',#10371,1.);
#3298=VECTOR('',#10372,1.);
#3299=VECTOR('',#10373,1.);
#3300=VECTOR('',#10376,1.);
#3301=VECTOR('',#10377,1.);
#3302=VECTOR('',#10378,1.);
#3303=VECTOR('',#10381,1.);
#3304=VECTOR('',#10382,1.);
#3305=VECTOR('',#10383,1.);
#3306=VECTOR('',#10386,1.);
#3307=VECTOR('',#10387,1.);
#3308=VECTOR('',#10388,1.);
#3309=VECTOR('',#10391,1.);
#3310=VECTOR('',#10392,1.);
#3311=VECTOR('',#10393,1.);
#3312=VECTOR('',#10396,1.);
#3313=VECTOR('',#10397,1.);
#3314=VECTOR('',#10408,0.32);
#3315=VECTOR('',#10415,0.6);
#3316=VECTOR('',#10432,0.475);
#3317=VECTOR('',#10437,0.5);
#3318=VECTOR('',#10442,0.485);
#3319=VECTOR('',#10451,0.31);
#3320=VECTOR('',#10456,0.3);
#3321=VECTOR('',#10461,0.27);
#3322=VECTOR('',#10466,1.);
#3323=VECTOR('',#10467,1.);
#3324=VECTOR('',#10468,1.);
#3325=VECTOR('',#10469,1.);
#3326=VECTOR('',#10472,1.);
#3327=VECTOR('',#10473,1.);
#3328=VECTOR('',#10474,1.);
#3329=VECTOR('',#10477,1.);
#3330=VECTOR('',#10478,1.);
#3331=VECTOR('',#10479,1.);
#3332=VECTOR('',#10482,1.);
#3333=VECTOR('',#10483,1.);
#3334=VECTOR('',#10484,1.);
#3335=VECTOR('',#10487,1.);
#3336=VECTOR('',#10488,1.);
#3337=VECTOR('',#10489,1.);
#3338=VECTOR('',#10492,1.);
#3339=VECTOR('',#10493,1.);
#3340=VECTOR('',#10504,0.225);
#3341=VECTOR('',#10509,0.215);
#3342=VECTOR('',#10518,0.45);
#3343=VECTOR('',#10527,1.);
#3344=VECTOR('',#10528,1.);
#3345=VECTOR('',#10529,1.);
#3346=VECTOR('',#10530,1.);
#3347=VECTOR('',#10533,1.);
#3348=VECTOR('',#10534,1.);
#3349=VECTOR('',#10535,1.);
#3350=VECTOR('',#10538,1.);
#3351=VECTOR('',#10539,1.);
#3352=VECTOR('',#10540,1.);
#3353=VECTOR('',#10543,1.);
#3354=VECTOR('',#10544,1.);
#3355=VECTOR('',#10545,1.);
#3356=VECTOR('',#10548,1.);
#3357=VECTOR('',#10549,1.);
#3358=VECTOR('',#10550,1.);
#3359=VECTOR('',#10553,1.);
#3360=VECTOR('',#10554,1.);
#3361=VECTOR('',#10571,0.325);
#3362=VECTOR('',#10576,0.35);
#3363=VECTOR('',#10581,0.335);
#3364=VECTOR('',#10590,0.21);
#3365=VECTOR('',#10593,0.2);
#3366=CIRCLE('',#7745,0.164999999999999);
#3367=CIRCLE('',#7746,0.164999999999999);
#3368=CIRCLE('',#7748,0.164999999999999);
#3369=CIRCLE('',#7749,0.164999999999999);
#3370=CIRCLE('',#7751,0.164999999999999);
#3371=CIRCLE('',#7752,0.164999999999999);
#3372=CIRCLE('',#7754,0.164999999999999);
#3373=CIRCLE('',#7755,0.164999999999999);
#3374=CIRCLE('',#7757,0.275);
#3375=CIRCLE('',#7758,0.275);
#3376=CIRCLE('',#7760,0.274999999999999);
#3377=CIRCLE('',#7761,0.274999999999999);
#3378=CIRCLE('',#7770,0.164999999999999);
#3379=CIRCLE('',#7771,0.164999999999999);
#3380=CIRCLE('',#7773,0.164999999999999);
#3381=CIRCLE('',#7774,0.164999999999999);
#3382=CIRCLE('',#7776,0.164999999999999);
#3383=CIRCLE('',#7777,0.164999999999999);
#3384=CIRCLE('',#7779,0.164999999999999);
#3385=CIRCLE('',#7780,0.164999999999999);
#3386=CIRCLE('',#7782,0.275);
#3387=CIRCLE('',#7783,0.275);
#3388=CIRCLE('',#7785,0.274999999999999);
#3389=CIRCLE('',#7786,0.274999999999999);
#3390=CIRCLE('',#7795,0.275);
#3391=CIRCLE('',#7796,0.275);
#3392=CIRCLE('',#7798,0.275);
#3393=CIRCLE('',#7799,0.275);
#3394=CIRCLE('',#7808,0.275);
#3395=CIRCLE('',#7809,0.275);
#3396=CIRCLE('',#7811,0.275);
#3397=CIRCLE('',#7812,0.275);
#3398=CIRCLE('',#7835,0.274999999999999);
#3399=CIRCLE('',#7836,0.274999999999999);
#3400=CIRCLE('',#7838,0.274999999999999);
#3401=CIRCLE('',#7839,0.274999999999999);
#3402=CIRCLE('',#7848,0.274999999999999);
#3403=CIRCLE('',#7849,0.274999999999999);
#3404=CIRCLE('',#7851,0.274999999999999);
#3405=CIRCLE('',#7852,0.274999999999999);
#3406=CIRCLE('',#7875,0.5);
#3407=CIRCLE('',#7876,0.5);
#3408=CIRCLE('',#7878,0.5);
#3409=CIRCLE('',#7879,0.5);
#3410=CIRCLE('',#7881,0.275);
#3411=CIRCLE('',#7883,0.5);
#3412=CIRCLE('',#7884,0.5);
#3413=CIRCLE('',#7886,0.5);
#3414=CIRCLE('',#7887,0.5);
#3415=CIRCLE('',#7889,0.275);
#3416=CIRCLE('',#7894,0.275);
#3417=CIRCLE('',#7896,0.275);
#3418=CIRCLE('',#7911,0.5);
#3419=CIRCLE('',#7912,0.5);
#3420=CIRCLE('',#7914,0.5);
#3421=CIRCLE('',#7915,0.5);
#3422=CIRCLE('',#7917,0.274999999999999);
#3423=CIRCLE('',#7919,0.5);
#3424=CIRCLE('',#7920,0.5);
#3425=CIRCLE('',#7922,0.5);
#3426=CIRCLE('',#7923,0.5);
#3427=CIRCLE('',#7925,0.274999999999999);
#3428=CIRCLE('',#7930,0.274999999999999);
#3429=CIRCLE('',#7932,0.274999999999999);
#3430=CIRCLE('',#7983,0.21);
#3431=CIRCLE('',#7984,0.21);
#3432=CIRCLE('',#7997,0.375);
#3433=CIRCLE('',#7998,0.375);
#3434=CIRCLE('',#8000,0.225);
#3435=CIRCLE('',#8002,0.375);
#3436=CIRCLE('',#8003,0.375);
#3437=CIRCLE('',#8005,0.225);
#3438=CIRCLE('',#8007,0.375);
#3439=CIRCLE('',#8008,0.375);
#3440=CIRCLE('',#8010,0.225);
#3441=CIRCLE('',#8012,0.375);
#3442=CIRCLE('',#8013,0.375);
#3443=CIRCLE('',#8015,0.225000000000001);
#3444=CIRCLE('',#8017,0.225);
#3445=CIRCLE('',#8019,0.225);
#3446=CIRCLE('',#8021,0.225);
#3447=CIRCLE('',#8023,0.225000000000001);
#3448=CIRCLE('',#8040,0.3);
#3449=CIRCLE('',#8042,0.35);
#3450=CIRCLE('',#8044,0.35);
#3451=CIRCLE('',#8046,0.32);
#3452=CIRCLE('',#8048,0.22);
#3453=CIRCLE('',#8050,0.1954);
#3454=CIRCLE('',#8052,0.1954);
#3455=CIRCLE('',#8054,0.16);
#3456=CIRCLE('',#8068,0.2117);
#3457=CIRCLE('',#8077,0.2117);
#3458=CIRCLE('',#8078,0.2117);
#3459=CIRCLE('',#8080,0.2117);
#3460=CIRCLE('',#8095,0.24505);
#3461=CIRCLE('',#8097,0.375);
#3462=CIRCLE('',#8099,0.425);
#3463=CIRCLE('',#8101,0.425);
#3464=CIRCLE('',#8103,0.395);
#3465=CIRCLE('',#8105,0.27);
#3466=CIRCLE('',#8107,0.24505);
#3467=CIRCLE('',#8112,0.164999999999999);
#3468=CIRCLE('',#8113,0.164999999999999);
#3469=CIRCLE('',#8115,0.164999999999999);
#3470=CIRCLE('',#8116,0.164999999999999);
#3471=CIRCLE('',#8118,0.25);
#3472=CIRCLE('',#8119,0.25);
#3473=CIRCLE('',#8121,0.274999999999999);
#3474=CIRCLE('',#8122,0.274999999999999);
#3475=CIRCLE('',#8124,0.274999999999999);
#3476=CIRCLE('',#8125,0.274999999999999);
#3477=CIRCLE('',#8127,0.274999999999999);
#3478=CIRCLE('',#8128,0.274999999999999);
#3479=CIRCLE('',#8130,0.274999999999999);
#3480=CIRCLE('',#8131,0.274999999999999);
#3481=CIRCLE('',#8133,0.274999999999999);
#3482=CIRCLE('',#8134,0.274999999999999);
#3483=CIRCLE('',#8136,0.275);
#3484=CIRCLE('',#8137,0.275);
#3485=CIRCLE('',#8139,0.275);
#3486=CIRCLE('',#8140,0.275);
#3487=CIRCLE('',#8142,0.274999999999999);
#3488=CIRCLE('',#8143,0.274999999999999);
#3489=CIRCLE('',#8145,0.274999999999999);
#3490=CIRCLE('',#8146,0.274999999999999);
#3491=CIRCLE('',#8148,0.274999999999999);
#3492=CIRCLE('',#8149,0.274999999999999);
#3493=CIRCLE('',#8151,0.274999999999999);
#3494=CIRCLE('',#8152,0.274999999999999);
#3495=CIRCLE('',#8154,0.274999999999999);
#3496=CIRCLE('',#8155,0.274999999999999);
#3497=CIRCLE('',#8157,0.274999999999999);
#3498=CIRCLE('',#8158,0.274999999999999);
#3499=CIRCLE('',#8160,0.275);
#3500=CIRCLE('',#8161,0.275);
#3501=CIRCLE('',#8163,0.275);
#3502=CIRCLE('',#8164,0.275);
#3503=CIRCLE('',#8166,0.274999999999999);
#3504=CIRCLE('',#8167,0.274999999999999);
#3505=CIRCLE('',#8176,0.329999999999998);
#3506=CIRCLE('',#8177,0.329999999999998);
#3507=CIRCLE('',#8179,1.5);
#3508=CIRCLE('',#8180,1.5);
#3509=CIRCLE('',#8185,0.225000000000001);
#3510=CIRCLE('',#8186,0.225000000000001);
#3511=CIRCLE('',#8188,0.225000000000001);
#3512=CIRCLE('',#8189,0.225000000000001);
#3513=CIRCLE('',#8201,0.21);
#3514=CIRCLE('',#8203,0.21);
#3515=CIRCLE('',#8204,0.21);
#3516=CIRCLE('',#8205,0.21);
#3517=CIRCLE('',#8207,0.21);
#3518=CIRCLE('',#8209,0.21);
#3519=CIRCLE('',#8210,0.21);
#3520=CIRCLE('',#8211,0.21);
#3521=CIRCLE('',#8213,0.21);
#3522=CIRCLE('',#8215,0.21);
#3523=CIRCLE('',#8216,0.21);
#3524=CIRCLE('',#8217,0.21);
#3525=CIRCLE('',#8219,0.21);
#3526=CIRCLE('',#8221,0.21);
#3527=CIRCLE('',#8222,0.21);
#3528=CIRCLE('',#8223,0.21);
#3529=CIRCLE('',#8265,0.285);
#3530=CIRCLE('',#8266,0.265);
#3531=CIRCLE('',#8268,0.265);
#3532=CIRCLE('',#8270,0.5);
#3533=CIRCLE('',#8272,0.5);
#3534=CIRCLE('',#8346,0.375);
#3535=CIRCLE('',#8348,0.425);
#3536=CIRCLE('',#8350,0.425);
#3537=CIRCLE('',#8352,0.395);
#3538=CIRCLE('',#8354,0.27);
#3539=CIRCLE('',#8356,0.24505);
#3540=CIRCLE('',#8358,0.24505);
#3541=CIRCLE('',#8360,0.2);
#3542=CIRCLE('',#8372,0.32);
#3543=CIRCLE('',#8373,0.32);
#3544=CIRCLE('',#8375,0.6);
#3545=CIRCLE('',#8376,0.6);
#3546=CIRCLE('',#8381,0.45);
#3547=CIRCLE('',#8383,0.5);
#3548=CIRCLE('',#8385,0.5);
#3549=CIRCLE('',#8387,0.47);
#3550=CIRCLE('',#8389,0.32);
#3551=CIRCLE('',#8391,0.2942);
#3552=CIRCLE('',#8393,0.2942);
#3553=CIRCLE('',#8395,0.24);
#3554=CIRCLE('',#8407,0.235);
#3555=CIRCLE('',#8408,0.215);
#3556=CIRCLE('',#8410,0.215);
#3557=CIRCLE('',#8412,0.45);
#3558=CIRCLE('',#8414,0.45);
#3559=CIRCLE('',#8426,0.1954);
#3560=CIRCLE('',#8428,0.3);
#3561=CIRCLE('',#8430,0.35);
#3562=CIRCLE('',#8432,0.35);
#3563=CIRCLE('',#8434,0.32);
#3564=CIRCLE('',#8436,0.22);
#3565=CIRCLE('',#8438,0.1954);
#3566=VERTEX_POINT('',#10692);
#3567=VERTEX_POINT('',#10694);
#3568=VERTEX_POINT('',#10698);
#3569=VERTEX_POINT('',#10700);
#3570=VERTEX_POINT('',#10704);
#3571=VERTEX_POINT('',#10706);
#3572=VERTEX_POINT('',#10710);
#3573=VERTEX_POINT('',#10712);
#3574=VERTEX_POINT('',#10716);
#3575=VERTEX_POINT('',#10718);
#3576=VERTEX_POINT('',#10722);
#3577=VERTEX_POINT('',#10724);
#3578=VERTEX_POINT('',#10728);
#3579=VERTEX_POINT('',#10729);
#3580=VERTEX_POINT('',#10731);
#3581=VERTEX_POINT('',#10733);
#3582=VERTEX_POINT('',#10737);
#3583=VERTEX_POINT('',#10739);
#3584=VERTEX_POINT('',#10743);
#3585=VERTEX_POINT('',#10745);
#3586=VERTEX_POINT('',#10755);
#3587=VERTEX_POINT('',#10757);
#3588=VERTEX_POINT('',#10761);
#3589=VERTEX_POINT('',#10763);
#3590=VERTEX_POINT('',#10767);
#3591=VERTEX_POINT('',#10769);
#3592=VERTEX_POINT('',#10773);
#3593=VERTEX_POINT('',#10775);
#3594=VERTEX_POINT('',#10779);
#3595=VERTEX_POINT('',#10781);
#3596=VERTEX_POINT('',#10785);
#3597=VERTEX_POINT('',#10787);
#3598=VERTEX_POINT('',#10791);
#3599=VERTEX_POINT('',#10792);
#3600=VERTEX_POINT('',#10794);
#3601=VERTEX_POINT('',#10796);
#3602=VERTEX_POINT('',#10800);
#3603=VERTEX_POINT('',#10802);
#3604=VERTEX_POINT('',#10806);
#3605=VERTEX_POINT('',#10808);
#3606=VERTEX_POINT('',#10818);
#3607=VERTEX_POINT('',#10820);
#3608=VERTEX_POINT('',#10824);
#3609=VERTEX_POINT('',#10826);
#3610=VERTEX_POINT('',#10830);
#3611=VERTEX_POINT('',#10831);
#3612=VERTEX_POINT('',#10833);
#3613=VERTEX_POINT('',#10835);
#3614=VERTEX_POINT('',#10839);
#3615=VERTEX_POINT('',#10841);
#3616=VERTEX_POINT('',#10845);
#3617=VERTEX_POINT('',#10847);
#3618=VERTEX_POINT('',#10857);
#3619=VERTEX_POINT('',#10859);
#3620=VERTEX_POINT('',#10863);
#3621=VERTEX_POINT('',#10865);
#3622=VERTEX_POINT('',#10869);
#3623=VERTEX_POINT('',#10870);
#3624=VERTEX_POINT('',#10872);
#3625=VERTEX_POINT('',#10874);
#3626=VERTEX_POINT('',#10878);
#3627=VERTEX_POINT('',#10880);
#3628=VERTEX_POINT('',#10884);
#3629=VERTEX_POINT('',#10886);
#3630=VERTEX_POINT('',#10896);
#3631=VERTEX_POINT('',#10897);
#3632=VERTEX_POINT('',#10899);
#3633=VERTEX_POINT('',#10901);
#3634=VERTEX_POINT('',#10905);
#3635=VERTEX_POINT('',#10907);
#3636=VERTEX_POINT('',#10911);
#3637=VERTEX_POINT('',#10913);
#3638=VERTEX_POINT('',#10923);
#3639=VERTEX_POINT('',#10924);
#3640=VERTEX_POINT('',#10926);
#3641=VERTEX_POINT('',#10928);
#3642=VERTEX_POINT('',#10932);
#3643=VERTEX_POINT('',#10934);
#3644=VERTEX_POINT('',#10938);
#3645=VERTEX_POINT('',#10940);
#3646=VERTEX_POINT('',#10950);
#3647=VERTEX_POINT('',#10952);
#3648=VERTEX_POINT('',#10956);
#3649=VERTEX_POINT('',#10958);
#3650=VERTEX_POINT('',#10962);
#3651=VERTEX_POINT('',#10963);
#3652=VERTEX_POINT('',#10965);
#3653=VERTEX_POINT('',#10967);
#3654=VERTEX_POINT('',#10971);
#3655=VERTEX_POINT('',#10973);
#3656=VERTEX_POINT('',#10977);
#3657=VERTEX_POINT('',#10979);
#3658=VERTEX_POINT('',#10989);
#3659=VERTEX_POINT('',#10991);
#3660=VERTEX_POINT('',#10995);
#3661=VERTEX_POINT('',#10997);
#3662=VERTEX_POINT('',#11001);
#3663=VERTEX_POINT('',#11002);
#3664=VERTEX_POINT('',#11004);
#3665=VERTEX_POINT('',#11006);
#3666=VERTEX_POINT('',#11010);
#3667=VERTEX_POINT('',#11012);
#3668=VERTEX_POINT('',#11016);
#3669=VERTEX_POINT('',#11018);
#3670=VERTEX_POINT('',#11028);
#3671=VERTEX_POINT('',#11029);
#3672=VERTEX_POINT('',#11031);
#3673=VERTEX_POINT('',#11033);
#3674=VERTEX_POINT('',#11037);
#3675=VERTEX_POINT('',#11039);
#3676=VERTEX_POINT('',#11043);
#3677=VERTEX_POINT('',#11045);
#3678=VERTEX_POINT('',#11055);
#3679=VERTEX_POINT('',#11056);
#3680=VERTEX_POINT('',#11058);
#3681=VERTEX_POINT('',#11060);
#3682=VERTEX_POINT('',#11064);
#3683=VERTEX_POINT('',#11066);
#3684=VERTEX_POINT('',#11070);
#3685=VERTEX_POINT('',#11072);
#3686=VERTEX_POINT('',#11082);
#3687=VERTEX_POINT('',#11083);
#3688=VERTEX_POINT('',#11085);
#3689=VERTEX_POINT('',#11087);
#3690=VERTEX_POINT('',#11096);
#3691=VERTEX_POINT('',#11099);
#3692=VERTEX_POINT('',#11100);
#3693=VERTEX_POINT('',#11102);
#3694=VERTEX_POINT('',#11104);
#3695=VERTEX_POINT('',#11113);
#3696=VERTEX_POINT('',#11116);
#3697=VERTEX_POINT('',#11118);
#3698=VERTEX_POINT('',#11125);
#3699=VERTEX_POINT('',#11127);
#3700=VERTEX_POINT('',#11131);
#3701=VERTEX_POINT('',#11135);
#3702=VERTEX_POINT('',#11139);
#3703=VERTEX_POINT('',#11140);
#3704=VERTEX_POINT('',#11145);
#3705=VERTEX_POINT('',#11149);
#3706=VERTEX_POINT('',#11157);
#3707=VERTEX_POINT('',#11158);
#3708=VERTEX_POINT('',#11160);
#3709=VERTEX_POINT('',#11162);
#3710=VERTEX_POINT('',#11166);
#3711=VERTEX_POINT('',#11168);
#3712=VERTEX_POINT('',#11172);
#3713=VERTEX_POINT('',#11174);
#3714=VERTEX_POINT('',#11184);
#3715=VERTEX_POINT('',#11185);
#3716=VERTEX_POINT('',#11187);
#3717=VERTEX_POINT('',#11189);
#3718=VERTEX_POINT('',#11198);
#3719=VERTEX_POINT('',#11201);
#3720=VERTEX_POINT('',#11202);
#3721=VERTEX_POINT('',#11204);
#3722=VERTEX_POINT('',#11206);
#3723=VERTEX_POINT('',#11215);
#3724=VERTEX_POINT('',#11218);
#3725=VERTEX_POINT('',#11220);
#3726=VERTEX_POINT('',#11227);
#3727=VERTEX_POINT('',#11229);
#3728=VERTEX_POINT('',#11233);
#3729=VERTEX_POINT('',#11237);
#3730=VERTEX_POINT('',#11241);
#3731=VERTEX_POINT('',#11242);
#3732=VERTEX_POINT('',#11247);
#3733=VERTEX_POINT('',#11251);
#3734=VERTEX_POINT('',#11259);
#3735=VERTEX_POINT('',#11260);
#3736=VERTEX_POINT('',#11262);
#3737=VERTEX_POINT('',#11264);
#3738=VERTEX_POINT('',#11268);
#3739=VERTEX_POINT('',#11270);
#3740=VERTEX_POINT('',#11274);
#3741=VERTEX_POINT('',#11276);
#3742=VERTEX_POINT('',#11286);
#3743=VERTEX_POINT('',#11287);
#3744=VERTEX_POINT('',#11289);
#3745=VERTEX_POINT('',#11291);
#3746=VERTEX_POINT('',#11295);
#3747=VERTEX_POINT('',#11297);
#3748=VERTEX_POINT('',#11301);
#3749=VERTEX_POINT('',#11303);
#3750=VERTEX_POINT('',#11307);
#3751=VERTEX_POINT('',#11309);
#3752=VERTEX_POINT('',#11313);
#3753=VERTEX_POINT('',#11315);
#3754=VERTEX_POINT('',#11319);
#3755=VERTEX_POINT('',#11321);
#3756=VERTEX_POINT('',#11325);
#3757=VERTEX_POINT('',#11327);
#3758=VERTEX_POINT('',#11331);
#3759=VERTEX_POINT('',#11333);
#3760=VERTEX_POINT('',#11337);
#3761=VERTEX_POINT('',#11339);
#3762=VERTEX_POINT('',#11343);
#3763=VERTEX_POINT('',#11344);
#3764=VERTEX_POINT('',#11346);
#3765=VERTEX_POINT('',#11348);
#3766=VERTEX_POINT('',#11352);
#3767=VERTEX_POINT('',#11354);
#3768=VERTEX_POINT('',#11358);
#3769=VERTEX_POINT('',#11360);
#3770=VERTEX_POINT('',#11364);
#3771=VERTEX_POINT('',#11366);
#3772=VERTEX_POINT('',#11370);
#3773=VERTEX_POINT('',#11372);
#3774=VERTEX_POINT('',#11376);
#3775=VERTEX_POINT('',#11378);
#3776=VERTEX_POINT('',#11382);
#3777=VERTEX_POINT('',#11384);
#3778=VERTEX_POINT('',#11388);
#3779=VERTEX_POINT('',#11390);
#3780=VERTEX_POINT('',#11394);
#3781=VERTEX_POINT('',#11396);
#3782=VERTEX_POINT('',#11400);
#3783=VERTEX_POINT('',#11401);
#3784=VERTEX_POINT('',#11403);
#3785=VERTEX_POINT('',#11405);
#3786=VERTEX_POINT('',#11409);
#3787=VERTEX_POINT('',#11411);
#3788=VERTEX_POINT('',#11415);
#3789=VERTEX_POINT('',#11417);
#3790=VERTEX_POINT('',#11421);
#3791=VERTEX_POINT('',#11423);
#3792=VERTEX_POINT('',#11427);
#3793=VERTEX_POINT('',#11429);
#3794=VERTEX_POINT('',#11433);
#3795=VERTEX_POINT('',#11435);
#3796=VERTEX_POINT('',#11439);
#3797=VERTEX_POINT('',#11441);
#3798=VERTEX_POINT('',#11445);
#3799=VERTEX_POINT('',#11447);
#3800=VERTEX_POINT('',#11451);
#3801=VERTEX_POINT('',#11453);
#3802=VERTEX_POINT('',#11457);
#3803=VERTEX_POINT('',#11458);
#3804=VERTEX_POINT('',#11460);
#3805=VERTEX_POINT('',#11462);
#3806=VERTEX_POINT('',#11466);
#3807=VERTEX_POINT('',#11468);
#3808=VERTEX_POINT('',#11472);
#3809=VERTEX_POINT('',#11474);
#3810=VERTEX_POINT('',#11478);
#3811=VERTEX_POINT('',#11480);
#3812=VERTEX_POINT('',#11484);
#3813=VERTEX_POINT('',#11486);
#3814=VERTEX_POINT('',#11490);
#3815=VERTEX_POINT('',#11492);
#3816=VERTEX_POINT('',#11496);
#3817=VERTEX_POINT('',#11498);
#3818=VERTEX_POINT('',#11502);
#3819=VERTEX_POINT('',#11504);
#3820=VERTEX_POINT('',#11508);
#3821=VERTEX_POINT('',#11510);
#3822=VERTEX_POINT('',#11514);
#3823=VERTEX_POINT('',#11516);
#3824=VERTEX_POINT('',#11520);
#3825=VERTEX_POINT('',#11522);
#3826=VERTEX_POINT('',#11526);
#3827=VERTEX_POINT('',#11528);
#3828=VERTEX_POINT('',#11535);
#3829=VERTEX_POINT('',#11537);
#3830=VERTEX_POINT('',#11544);
#3831=VERTEX_POINT('',#11546);
#3832=VERTEX_POINT('',#11559);
#3833=VERTEX_POINT('',#11561);
#3834=VERTEX_POINT('',#11565);
#3835=VERTEX_POINT('',#11568);
#3836=VERTEX_POINT('',#11570);
#3837=VERTEX_POINT('',#11574);
#3838=VERTEX_POINT('',#11577);
#3839=VERTEX_POINT('',#11579);
#3840=VERTEX_POINT('',#11583);
#3841=VERTEX_POINT('',#11586);
#3842=VERTEX_POINT('',#11588);
#3843=VERTEX_POINT('',#11592);
#3844=VERTEX_POINT('',#11595);
#3845=VERTEX_POINT('',#11599);
#3846=VERTEX_POINT('',#11603);
#3847=VERTEX_POINT('',#11607);
#3848=VERTEX_POINT('',#11611);
#3849=VERTEX_POINT('',#11612);
#3850=VERTEX_POINT('',#11614);
#3851=VERTEX_POINT('',#11616);
#3852=VERTEX_POINT('',#11620);
#3853=VERTEX_POINT('',#11622);
#3854=VERTEX_POINT('',#11626);
#3855=VERTEX_POINT('',#11628);
#3856=VERTEX_POINT('',#11632);
#3857=VERTEX_POINT('',#11634);
#3858=VERTEX_POINT('',#11638);
#3859=VERTEX_POINT('',#11640);
#3860=VERTEX_POINT('',#11644);
#3861=VERTEX_POINT('',#11646);
#3862=VERTEX_POINT('',#11650);
#3863=VERTEX_POINT('',#11652);
#3864=VERTEX_POINT('',#11656);
#3865=VERTEX_POINT('',#11658);
#3866=VERTEX_POINT('',#11662);
#3867=VERTEX_POINT('',#11664);
#3868=VERTEX_POINT('',#11668);
#3869=VERTEX_POINT('',#11670);
#3870=VERTEX_POINT('',#11674);
#3871=VERTEX_POINT('',#11676);
#3872=VERTEX_POINT('',#11686);
#3873=VERTEX_POINT('',#11689);
#3874=VERTEX_POINT('',#11693);
#3875=VERTEX_POINT('',#11697);
#3876=VERTEX_POINT('',#11701);
#3877=VERTEX_POINT('',#11704);
#3878=VERTEX_POINT('',#11708);
#3879=VERTEX_POINT('',#11712);
#3880=VERTEX_POINT('',#11717);
#3881=VERTEX_POINT('',#11718);
#3882=VERTEX_POINT('',#11720);
#3883=VERTEX_POINT('',#11722);
#3884=VERTEX_POINT('',#11726);
#3885=VERTEX_POINT('',#11728);
#3886=VERTEX_POINT('',#11732);
#3887=VERTEX_POINT('',#11734);
#3888=VERTEX_POINT('',#11738);
#3889=VERTEX_POINT('',#11740);
#3890=VERTEX_POINT('',#11744);
#3891=VERTEX_POINT('',#11746);
#3892=VERTEX_POINT('',#11756);
#3893=VERTEX_POINT('',#11757);
#3894=VERTEX_POINT('',#11759);
#3895=VERTEX_POINT('',#11761);
#3896=VERTEX_POINT('',#11765);
#3897=VERTEX_POINT('',#11767);
#3898=VERTEX_POINT('',#11771);
#3899=VERTEX_POINT('',#11773);
#3900=VERTEX_POINT('',#11776);
#3901=VERTEX_POINT('',#11779);
#3902=VERTEX_POINT('',#11781);
#3903=VERTEX_POINT('',#11783);
#3904=VERTEX_POINT('',#11785);
#3905=VERTEX_POINT('',#11787);
#3906=VERTEX_POINT('',#11789);
#3907=VERTEX_POINT('',#11793);
#3908=VERTEX_POINT('',#11797);
#3909=VERTEX_POINT('',#11801);
#3910=VERTEX_POINT('',#11803);
#3911=VERTEX_POINT('',#11805);
#3912=VERTEX_POINT('',#11807);
#3913=VERTEX_POINT('',#11813);
#3914=VERTEX_POINT('',#11815);
#3915=VERTEX_POINT('',#11819);
#3916=VERTEX_POINT('',#11822);
#3917=VERTEX_POINT('',#11824);
#3918=VERTEX_POINT('',#11836);
#3919=VERTEX_POINT('',#11837);
#3920=VERTEX_POINT('',#11839);
#3921=VERTEX_POINT('',#11841);
#3922=VERTEX_POINT('',#11845);
#3923=VERTEX_POINT('',#11847);
#3924=VERTEX_POINT('',#11851);
#3925=VERTEX_POINT('',#11853);
#3926=VERTEX_POINT('',#11857);
#3927=VERTEX_POINT('',#11859);
#3928=VERTEX_POINT('',#11863);
#3929=VERTEX_POINT('',#11865);
#3930=VERTEX_POINT('',#11874);
#3931=VERTEX_POINT('',#11877);
#3932=VERTEX_POINT('',#11880);
#3933=VERTEX_POINT('',#11884);
#3934=VERTEX_POINT('',#11888);
#3935=VERTEX_POINT('',#11892);
#3936=VERTEX_POINT('',#11895);
#3937=VERTEX_POINT('',#11903);
#3938=VERTEX_POINT('',#11905);
#3939=VERTEX_POINT('',#11909);
#3940=VERTEX_POINT('',#11911);
#3941=VERTEX_POINT('',#11915);
#3942=VERTEX_POINT('',#11917);
#3943=VERTEX_POINT('',#11921);
#3944=VERTEX_POINT('',#11923);
#3945=VERTEX_POINT('',#11927);
#3946=VERTEX_POINT('',#11929);
#3947=VERTEX_POINT('',#11933);
#3948=VERTEX_POINT('',#11935);
#3949=VERTEX_POINT('',#11939);
#3950=VERTEX_POINT('',#11941);
#3951=VERTEX_POINT('',#11945);
#3952=VERTEX_POINT('',#11947);
#3953=VERTEX_POINT('',#11951);
#3954=VERTEX_POINT('',#11953);
#3955=VERTEX_POINT('',#11957);
#3956=VERTEX_POINT('',#11959);
#3957=VERTEX_POINT('',#11963);
#3958=VERTEX_POINT('',#11965);
#3959=VERTEX_POINT('',#11969);
#3960=VERTEX_POINT('',#11971);
#3961=VERTEX_POINT('',#11975);
#3962=VERTEX_POINT('',#11977);
#3963=VERTEX_POINT('',#11981);
#3964=VERTEX_POINT('',#11983);
#3965=VERTEX_POINT('',#11987);
#3966=VERTEX_POINT('',#11989);
#3967=VERTEX_POINT('',#11993);
#3968=VERTEX_POINT('',#11995);
#3969=VERTEX_POINT('',#11999);
#3970=VERTEX_POINT('',#12001);
#3971=VERTEX_POINT('',#12005);
#3972=VERTEX_POINT('',#12007);
#3973=VERTEX_POINT('',#12011);
#3974=VERTEX_POINT('',#12013);
#3975=VERTEX_POINT('',#12017);
#3976=VERTEX_POINT('',#12018);
#3977=VERTEX_POINT('',#12020);
#3978=VERTEX_POINT('',#12022);
#3979=VERTEX_POINT('',#12026);
#3980=VERTEX_POINT('',#12028);
#3981=VERTEX_POINT('',#12032);
#3982=VERTEX_POINT('',#12034);
#3983=VERTEX_POINT('',#12044);
#3984=VERTEX_POINT('',#12046);
#3985=VERTEX_POINT('',#12050);
#3986=VERTEX_POINT('',#12052);
#3987=VERTEX_POINT('',#12059);
#3988=VERTEX_POINT('',#12061);
#3989=VERTEX_POINT('',#12065);
#3990=VERTEX_POINT('',#12067);
#3991=VERTEX_POINT('',#12071);
#3992=VERTEX_POINT('',#12072);
#3993=VERTEX_POINT('',#12074);
#3994=VERTEX_POINT('',#12076);
#3995=VERTEX_POINT('',#12080);
#3996=VERTEX_POINT('',#12082);
#3997=VERTEX_POINT('',#12086);
#3998=VERTEX_POINT('',#12088);
#3999=VERTEX_POINT('',#12092);
#4000=VERTEX_POINT('',#12094);
#4001=VERTEX_POINT('',#12098);
#4002=VERTEX_POINT('',#12100);
#4003=VERTEX_POINT('',#12111);
#4004=VERTEX_POINT('',#12112);
#4005=VERTEX_POINT('',#12116);
#4006=VERTEX_POINT('',#12118);
#4007=VERTEX_POINT('',#12120);
#4008=VERTEX_POINT('',#12123);
#4009=VERTEX_POINT('',#12127);
#4010=VERTEX_POINT('',#12128);
#4011=VERTEX_POINT('',#12132);
#4012=VERTEX_POINT('',#12134);
#4013=VERTEX_POINT('',#12136);
#4014=VERTEX_POINT('',#12139);
#4015=VERTEX_POINT('',#12143);
#4016=VERTEX_POINT('',#12144);
#4017=VERTEX_POINT('',#12148);
#4018=VERTEX_POINT('',#12150);
#4019=VERTEX_POINT('',#12152);
#4020=VERTEX_POINT('',#12155);
#4021=VERTEX_POINT('',#12159);
#4022=VERTEX_POINT('',#12160);
#4023=VERTEX_POINT('',#12164);
#4024=VERTEX_POINT('',#12166);
#4025=VERTEX_POINT('',#12168);
#4026=VERTEX_POINT('',#12171);
#4027=VERTEX_POINT('',#12176);
#4028=VERTEX_POINT('',#12178);
#4029=VERTEX_POINT('',#12180);
#4030=VERTEX_POINT('',#12182);
#4031=VERTEX_POINT('',#12187);
#4032=VERTEX_POINT('',#12189);
#4033=VERTEX_POINT('',#12191);
#4034=VERTEX_POINT('',#12193);
#4035=VERTEX_POINT('',#12197);
#4036=VERTEX_POINT('',#12199);
#4037=VERTEX_POINT('',#12201);
#4038=VERTEX_POINT('',#12203);
#4039=VERTEX_POINT('',#12206);
#4040=VERTEX_POINT('',#12208);
#4041=VERTEX_POINT('',#12210);
#4042=VERTEX_POINT('',#12212);
#4043=VERTEX_POINT('',#12216);
#4044=VERTEX_POINT('',#12220);
#4045=VERTEX_POINT('',#12224);
#4046=VERTEX_POINT('',#12228);
#4047=VERTEX_POINT('',#12234);
#4048=VERTEX_POINT('',#12238);
#4049=VERTEX_POINT('',#12242);
#4050=VERTEX_POINT('',#12246);
#4051=VERTEX_POINT('',#12254);
#4052=VERTEX_POINT('',#12255);
#4053=VERTEX_POINT('',#12257);
#4054=VERTEX_POINT('',#12259);
#4055=VERTEX_POINT('',#12263);
#4056=VERTEX_POINT('',#12265);
#4057=VERTEX_POINT('',#12269);
#4058=VERTEX_POINT('',#12271);
#4059=VERTEX_POINT('',#12275);
#4060=VERTEX_POINT('',#12277);
#4061=VERTEX_POINT('',#12281);
#4062=VERTEX_POINT('',#12283);
#4063=VERTEX_POINT('',#12287);
#4064=VERTEX_POINT('',#12289);
#4065=VERTEX_POINT('',#12293);
#4066=VERTEX_POINT('',#12295);
#4067=VERTEX_POINT('',#12305);
#4068=VERTEX_POINT('',#12306);
#4069=VERTEX_POINT('',#12308);
#4070=VERTEX_POINT('',#12310);
#4071=VERTEX_POINT('',#12314);
#4072=VERTEX_POINT('',#12316);
#4073=VERTEX_POINT('',#12320);
#4074=VERTEX_POINT('',#12322);
#4075=VERTEX_POINT('',#12326);
#4076=VERTEX_POINT('',#12328);
#4077=VERTEX_POINT('',#12332);
#4078=VERTEX_POINT('',#12334);
#4079=VERTEX_POINT('',#12338);
#4080=VERTEX_POINT('',#12340);
#4081=VERTEX_POINT('',#12344);
#4082=VERTEX_POINT('',#12346);
#4083=VERTEX_POINT('',#12359);
#4084=VERTEX_POINT('',#12361);
#4085=VERTEX_POINT('',#12365);
#4086=VERTEX_POINT('',#12369);
#4087=VERTEX_POINT('',#12372);
#4088=VERTEX_POINT('',#12448);
#4089=VERTEX_POINT('',#12451);
#4090=VERTEX_POINT('',#12455);
#4091=VERTEX_POINT('',#12459);
#4092=VERTEX_POINT('',#12463);
#4093=VERTEX_POINT('',#12466);
#4094=VERTEX_POINT('',#12470);
#4095=VERTEX_POINT('',#12474);
#4096=VERTEX_POINT('',#12479);
#4097=VERTEX_POINT('',#12480);
#4098=VERTEX_POINT('',#12482);
#4099=VERTEX_POINT('',#12484);
#4100=VERTEX_POINT('',#12488);
#4101=VERTEX_POINT('',#12490);
#4102=VERTEX_POINT('',#12494);
#4103=VERTEX_POINT('',#12496);
#4104=VERTEX_POINT('',#12500);
#4105=VERTEX_POINT('',#12502);
#4106=VERTEX_POINT('',#12506);
#4107=VERTEX_POINT('',#12508);
#4108=VERTEX_POINT('',#12518);
#4109=VERTEX_POINT('',#12520);
#4110=VERTEX_POINT('',#12524);
#4111=VERTEX_POINT('',#12526);
#4112=VERTEX_POINT('',#12533);
#4113=VERTEX_POINT('',#12536);
#4114=VERTEX_POINT('',#12540);
#4115=VERTEX_POINT('',#12544);
#4116=VERTEX_POINT('',#12548);
#4117=VERTEX_POINT('',#12551);
#4118=VERTEX_POINT('',#12555);
#4119=VERTEX_POINT('',#12559);
#4120=VERTEX_POINT('',#12564);
#4121=VERTEX_POINT('',#12565);
#4122=VERTEX_POINT('',#12567);
#4123=VERTEX_POINT('',#12569);
#4124=VERTEX_POINT('',#12573);
#4125=VERTEX_POINT('',#12575);
#4126=VERTEX_POINT('',#12579);
#4127=VERTEX_POINT('',#12581);
#4128=VERTEX_POINT('',#12585);
#4129=VERTEX_POINT('',#12587);
#4130=VERTEX_POINT('',#12591);
#4131=VERTEX_POINT('',#12593);
#4132=VERTEX_POINT('',#12603);
#4133=VERTEX_POINT('',#12605);
#4134=VERTEX_POINT('',#12609);
#4135=VERTEX_POINT('',#12613);
#4136=VERTEX_POINT('',#12616);
#4137=VERTEX_POINT('',#12622);
#4138=VERTEX_POINT('',#12623);
#4139=VERTEX_POINT('',#12625);
#4140=VERTEX_POINT('',#12627);
#4141=VERTEX_POINT('',#12631);
#4142=VERTEX_POINT('',#12633);
#4143=VERTEX_POINT('',#12637);
#4144=VERTEX_POINT('',#12639);
#4145=VERTEX_POINT('',#12643);
#4146=VERTEX_POINT('',#12645);
#4147=VERTEX_POINT('',#12649);
#4148=VERTEX_POINT('',#12651);
#4149=VERTEX_POINT('',#12660);
#4150=VERTEX_POINT('',#12663);
#4151=VERTEX_POINT('',#12666);
#4152=VERTEX_POINT('',#12670);
#4153=VERTEX_POINT('',#12674);
#4154=VERTEX_POINT('',#12678);
#4155=VERTEX_POINT('',#12681);
#4156=EDGE_CURVE('',#3566,#3566,#3366,.T.);
#4157=EDGE_CURVE('',#3566,#3567,#1948,.T.);
#4158=EDGE_CURVE('',#3567,#3567,#3367,.T.);
#4159=EDGE_CURVE('',#3568,#3568,#3368,.T.);
#4160=EDGE_CURVE('',#3568,#3569,#1949,.T.);
#4161=EDGE_CURVE('',#3569,#3569,#3369,.T.);
#4162=EDGE_CURVE('',#3570,#3570,#3370,.T.);
#4163=EDGE_CURVE('',#3570,#3571,#1950,.T.);
#4164=EDGE_CURVE('',#3571,#3571,#3371,.T.);
#4165=EDGE_CURVE('',#3572,#3572,#3372,.T.);
#4166=EDGE_CURVE('',#3572,#3573,#1951,.T.);
#4167=EDGE_CURVE('',#3573,#3573,#3373,.T.);
#4168=EDGE_CURVE('',#3574,#3574,#3374,.T.);
#4169=EDGE_CURVE('',#3574,#3575,#1952,.T.);
#4170=EDGE_CURVE('',#3575,#3575,#3375,.T.);
#4171=EDGE_CURVE('',#3576,#3576,#3376,.T.);
#4172=EDGE_CURVE('',#3576,#3577,#1953,.T.);
#4173=EDGE_CURVE('',#3577,#3577,#3377,.T.);
#4174=EDGE_CURVE('',#3578,#3579,#1954,.T.);
#4175=EDGE_CURVE('',#3579,#3580,#1955,.T.);
#4176=EDGE_CURVE('',#3581,#3580,#1956,.T.);
#4177=EDGE_CURVE('',#3578,#3581,#1957,.T.);
#4178=EDGE_CURVE('',#3582,#3578,#1958,.T.);
#4179=EDGE_CURVE('',#3583,#3581,#1959,.T.);
#4180=EDGE_CURVE('',#3582,#3583,#1960,.T.);
#4181=EDGE_CURVE('',#3584,#3582,#1961,.T.);
#4182=EDGE_CURVE('',#3585,#3583,#1962,.T.);
#4183=EDGE_CURVE('',#3584,#3585,#1963,.T.);
#4184=EDGE_CURVE('',#3579,#3584,#1964,.T.);
#4185=EDGE_CURVE('',#3580,#3585,#1965,.T.);
#4186=EDGE_CURVE('',#3586,#3586,#3378,.T.);
#4187=EDGE_CURVE('',#3586,#3587,#1966,.T.);
#4188=EDGE_CURVE('',#3587,#3587,#3379,.T.);
#4189=EDGE_CURVE('',#3588,#3588,#3380,.T.);
#4190=EDGE_CURVE('',#3588,#3589,#1967,.T.);
#4191=EDGE_CURVE('',#3589,#3589,#3381,.T.);
#4192=EDGE_CURVE('',#3590,#3590,#3382,.T.);
#4193=EDGE_CURVE('',#3590,#3591,#1968,.T.);
#4194=EDGE_CURVE('',#3591,#3591,#3383,.T.);
#4195=EDGE_CURVE('',#3592,#3592,#3384,.T.);
#4196=EDGE_CURVE('',#3592,#3593,#1969,.T.);
#4197=EDGE_CURVE('',#3593,#3593,#3385,.T.);
#4198=EDGE_CURVE('',#3594,#3594,#3386,.T.);
#4199=EDGE_CURVE('',#3594,#3595,#1970,.T.);
#4200=EDGE_CURVE('',#3595,#3595,#3387,.T.);
#4201=EDGE_CURVE('',#3596,#3596,#3388,.T.);
#4202=EDGE_CURVE('',#3596,#3597,#1971,.T.);
#4203=EDGE_CURVE('',#3597,#3597,#3389,.T.);
#4204=EDGE_CURVE('',#3598,#3599,#1972,.T.);
#4205=EDGE_CURVE('',#3599,#3600,#1973,.T.);
#4206=EDGE_CURVE('',#3601,#3600,#1974,.T.);
#4207=EDGE_CURVE('',#3598,#3601,#1975,.T.);
#4208=EDGE_CURVE('',#3602,#3598,#1976,.T.);
#4209=EDGE_CURVE('',#3603,#3601,#1977,.T.);
#4210=EDGE_CURVE('',#3602,#3603,#1978,.T.);
#4211=EDGE_CURVE('',#3604,#3602,#1979,.T.);
#4212=EDGE_CURVE('',#3605,#3603,#1980,.T.);
#4213=EDGE_CURVE('',#3604,#3605,#1981,.T.);
#4214=EDGE_CURVE('',#3599,#3604,#1982,.T.);
#4215=EDGE_CURVE('',#3600,#3605,#1983,.T.);
#4216=EDGE_CURVE('',#3606,#3606,#3390,.T.);
#4217=EDGE_CURVE('',#3606,#3607,#1984,.T.);
#4218=EDGE_CURVE('',#3607,#3607,#3391,.T.);
#4219=EDGE_CURVE('',#3608,#3608,#3392,.T.);
#4220=EDGE_CURVE('',#3608,#3609,#1985,.T.);
#4221=EDGE_CURVE('',#3609,#3609,#3393,.T.);
#4222=EDGE_CURVE('',#3610,#3611,#1986,.T.);
#4223=EDGE_CURVE('',#3611,#3612,#1987,.T.);
#4224=EDGE_CURVE('',#3613,#3612,#1988,.T.);
#4225=EDGE_CURVE('',#3610,#3613,#1989,.T.);
#4226=EDGE_CURVE('',#3614,#3610,#1990,.T.);
#4227=EDGE_CURVE('',#3615,#3613,#1991,.T.);
#4228=EDGE_CURVE('',#3614,#3615,#1992,.T.);
#4229=EDGE_CURVE('',#3616,#3614,#1993,.T.);
#4230=EDGE_CURVE('',#3617,#3615,#1994,.T.);
#4231=EDGE_CURVE('',#3616,#3617,#1995,.T.);
#4232=EDGE_CURVE('',#3611,#3616,#1996,.T.);
#4233=EDGE_CURVE('',#3612,#3617,#1997,.T.);
#4234=EDGE_CURVE('',#3618,#3618,#3394,.T.);
#4235=EDGE_CURVE('',#3618,#3619,#1998,.T.);
#4236=EDGE_CURVE('',#3619,#3619,#3395,.T.);
#4237=EDGE_CURVE('',#3620,#3620,#3396,.T.);
#4238=EDGE_CURVE('',#3620,#3621,#1999,.T.);
#4239=EDGE_CURVE('',#3621,#3621,#3397,.T.);
#4240=EDGE_CURVE('',#3622,#3623,#2000,.T.);
#4241=EDGE_CURVE('',#3623,#3624,#2001,.T.);
#4242=EDGE_CURVE('',#3625,#3624,#2002,.T.);
#4243=EDGE_CURVE('',#3622,#3625,#2003,.T.);
#4244=EDGE_CURVE('',#3626,#3622,#2004,.T.);
#4245=EDGE_CURVE('',#3627,#3625,#2005,.T.);
#4246=EDGE_CURVE('',#3626,#3627,#2006,.T.);
#4247=EDGE_CURVE('',#3628,#3626,#2007,.T.);
#4248=EDGE_CURVE('',#3629,#3627,#2008,.T.);
#4249=EDGE_CURVE('',#3628,#3629,#2009,.T.);
#4250=EDGE_CURVE('',#3623,#3628,#2010,.T.);
#4251=EDGE_CURVE('',#3624,#3629,#2011,.T.);
#4252=EDGE_CURVE('',#3630,#3631,#2012,.T.);
#4253=EDGE_CURVE('',#3631,#3632,#2013,.T.);
#4254=EDGE_CURVE('',#3633,#3632,#2014,.T.);
#4255=EDGE_CURVE('',#3630,#3633,#2015,.T.);
#4256=EDGE_CURVE('',#3634,#3630,#2016,.T.);
#4257=EDGE_CURVE('',#3635,#3633,#2017,.T.);
#4258=EDGE_CURVE('',#3634,#3635,#2018,.T.);
#4259=EDGE_CURVE('',#3636,#3634,#2019,.T.);
#4260=EDGE_CURVE('',#3637,#3635,#2020,.T.);
#4261=EDGE_CURVE('',#3636,#3637,#2021,.T.);
#4262=EDGE_CURVE('',#3631,#3636,#2022,.T.);
#4263=EDGE_CURVE('',#3632,#3637,#2023,.T.);
#4264=EDGE_CURVE('',#3638,#3639,#2024,.T.);
#4265=EDGE_CURVE('',#3639,#3640,#2025,.T.);
#4266=EDGE_CURVE('',#3641,#3640,#2026,.T.);
#4267=EDGE_CURVE('',#3638,#3641,#2027,.T.);
#4268=EDGE_CURVE('',#3642,#3638,#2028,.T.);
#4269=EDGE_CURVE('',#3643,#3641,#2029,.T.);
#4270=EDGE_CURVE('',#3642,#3643,#2030,.T.);
#4271=EDGE_CURVE('',#3644,#3642,#2031,.T.);
#4272=EDGE_CURVE('',#3645,#3643,#2032,.T.);
#4273=EDGE_CURVE('',#3644,#3645,#2033,.T.);
#4274=EDGE_CURVE('',#3639,#3644,#2034,.T.);
#4275=EDGE_CURVE('',#3640,#3645,#2035,.T.);
#4276=EDGE_CURVE('',#3646,#3646,#3398,.T.);
#4277=EDGE_CURVE('',#3646,#3647,#2036,.T.);
#4278=EDGE_CURVE('',#3647,#3647,#3399,.T.);
#4279=EDGE_CURVE('',#3648,#3648,#3400,.T.);
#4280=EDGE_CURVE('',#3648,#3649,#2037,.T.);
#4281=EDGE_CURVE('',#3649,#3649,#3401,.T.);
#4282=EDGE_CURVE('',#3650,#3651,#2038,.T.);
#4283=EDGE_CURVE('',#3651,#3652,#2039,.T.);
#4284=EDGE_CURVE('',#3653,#3652,#2040,.T.);
#4285=EDGE_CURVE('',#3650,#3653,#2041,.T.);
#4286=EDGE_CURVE('',#3654,#3650,#2042,.T.);
#4287=EDGE_CURVE('',#3655,#3653,#2043,.T.);
#4288=EDGE_CURVE('',#3654,#3655,#2044,.T.);
#4289=EDGE_CURVE('',#3656,#3654,#2045,.T.);
#4290=EDGE_CURVE('',#3657,#3655,#2046,.T.);
#4291=EDGE_CURVE('',#3656,#3657,#2047,.T.);
#4292=EDGE_CURVE('',#3651,#3656,#2048,.T.);
#4293=EDGE_CURVE('',#3652,#3657,#2049,.T.);
#4294=EDGE_CURVE('',#3658,#3658,#3402,.T.);
#4295=EDGE_CURVE('',#3658,#3659,#2050,.T.);
#4296=EDGE_CURVE('',#3659,#3659,#3403,.T.);
#4297=EDGE_CURVE('',#3660,#3660,#3404,.T.);
#4298=EDGE_CURVE('',#3660,#3661,#2051,.T.);
#4299=EDGE_CURVE('',#3661,#3661,#3405,.T.);
#4300=EDGE_CURVE('',#3662,#3663,#2052,.T.);
#4301=EDGE_CURVE('',#3663,#3664,#2053,.T.);
#4302=EDGE_CURVE('',#3665,#3664,#2054,.T.);
#4303=EDGE_CURVE('',#3662,#3665,#2055,.T.);
#4304=EDGE_CURVE('',#3666,#3662,#2056,.T.);
#4305=EDGE_CURVE('',#3667,#3665,#2057,.T.);
#4306=EDGE_CURVE('',#3666,#3667,#2058,.T.);
#4307=EDGE_CURVE('',#3668,#3666,#2059,.T.);
#4308=EDGE_CURVE('',#3669,#3667,#2060,.T.);
#4309=EDGE_CURVE('',#3668,#3669,#2061,.T.);
#4310=EDGE_CURVE('',#3663,#3668,#2062,.T.);
#4311=EDGE_CURVE('',#3664,#3669,#2063,.T.);
#4312=EDGE_CURVE('',#3670,#3671,#2064,.T.);
#4313=EDGE_CURVE('',#3671,#3672,#2065,.T.);
#4314=EDGE_CURVE('',#3673,#3672,#2066,.T.);
#4315=EDGE_CURVE('',#3670,#3673,#2067,.T.);
#4316=EDGE_CURVE('',#3674,#3670,#2068,.T.);
#4317=EDGE_CURVE('',#3675,#3673,#2069,.T.);
#4318=EDGE_CURVE('',#3674,#3675,#2070,.T.);
#4319=EDGE_CURVE('',#3676,#3674,#2071,.T.);
#4320=EDGE_CURVE('',#3677,#3675,#2072,.T.);
#4321=EDGE_CURVE('',#3676,#3677,#2073,.T.);
#4322=EDGE_CURVE('',#3671,#3676,#2074,.T.);
#4323=EDGE_CURVE('',#3672,#3677,#2075,.T.);
#4324=EDGE_CURVE('',#3678,#3679,#2076,.T.);
#4325=EDGE_CURVE('',#3679,#3680,#2077,.T.);
#4326=EDGE_CURVE('',#3681,#3680,#2078,.T.);
#4327=EDGE_CURVE('',#3678,#3681,#2079,.T.);
#4328=EDGE_CURVE('',#3682,#3678,#2080,.T.);
#4329=EDGE_CURVE('',#3683,#3681,#2081,.T.);
#4330=EDGE_CURVE('',#3682,#3683,#2082,.T.);
#4331=EDGE_CURVE('',#3684,#3682,#2083,.T.);
#4332=EDGE_CURVE('',#3685,#3683,#2084,.T.);
#4333=EDGE_CURVE('',#3684,#3685,#2085,.T.);
#4334=EDGE_CURVE('',#3679,#3684,#2086,.T.);
#4335=EDGE_CURVE('',#3680,#3685,#2087,.T.);
#4336=EDGE_CURVE('',#3686,#3687,#2088,.T.);
#4337=EDGE_CURVE('',#3688,#3687,#3406,.T.);
#4338=EDGE_CURVE('',#3689,#3688,#2089,.T.);
#4339=EDGE_CURVE('',#3686,#3689,#3407,.T.);
#4340=EDGE_CURVE('',#3686,#3687,#2090,.T.);
#4341=EDGE_CURVE('',#3689,#3686,#3408,.T.);
#4342=EDGE_CURVE('',#3689,#3688,#2091,.T.);
#4343=EDGE_CURVE('',#3687,#3688,#3409,.T.);
#4344=EDGE_CURVE('',#3690,#3690,#3410,.T.);
#4345=EDGE_CURVE('',#3691,#3692,#2092,.T.);
#4346=EDGE_CURVE('',#3693,#3692,#3411,.T.);
#4347=EDGE_CURVE('',#3694,#3693,#2093,.T.);
#4348=EDGE_CURVE('',#3691,#3694,#3412,.T.);
#4349=EDGE_CURVE('',#3691,#3692,#2094,.T.);
#4350=EDGE_CURVE('',#3694,#3691,#3413,.T.);
#4351=EDGE_CURVE('',#3694,#3693,#2095,.T.);
#4352=EDGE_CURVE('',#3692,#3693,#3414,.T.);
#4353=EDGE_CURVE('',#3695,#3695,#3415,.T.);
#4354=EDGE_CURVE('',#3692,#3696,#2096,.T.);
#4355=EDGE_CURVE('',#3696,#3697,#2097,.T.);
#4356=EDGE_CURVE('',#3697,#3693,#2098,.T.);
#4357=EDGE_CURVE('',#3687,#3692,#2099,.T.);
#4358=EDGE_CURVE('',#3693,#3688,#2100,.T.);
#4359=EDGE_CURVE('',#3688,#3698,#2101,.T.);
#4360=EDGE_CURVE('',#3698,#3699,#2102,.T.);
#4361=EDGE_CURVE('',#3699,#3687,#2103,.T.);
#4362=EDGE_CURVE('',#3700,#3700,#3416,.T.);
#4363=EDGE_CURVE('',#3700,#3690,#2104,.T.);
#4364=EDGE_CURVE('',#3701,#3701,#3417,.T.);
#4365=EDGE_CURVE('',#3701,#3695,#2105,.T.);
#4366=EDGE_CURVE('',#3702,#3703,#2106,.T.);
#4367=EDGE_CURVE('',#3703,#3697,#2107,.T.);
#4368=EDGE_CURVE('',#3702,#3696,#2108,.T.);
#4369=EDGE_CURVE('',#3704,#3702,#2109,.T.);
#4370=EDGE_CURVE('',#3704,#3699,#2110,.T.);
#4371=EDGE_CURVE('',#3705,#3704,#2111,.T.);
#4372=EDGE_CURVE('',#3705,#3698,#2112,.T.);
#4373=EDGE_CURVE('',#3703,#3705,#2113,.T.);
#4374=EDGE_CURVE('',#3706,#3707,#2114,.T.);
#4375=EDGE_CURVE('',#3707,#3708,#2115,.T.);
#4376=EDGE_CURVE('',#3709,#3708,#2116,.T.);
#4377=EDGE_CURVE('',#3706,#3709,#2117,.T.);
#4378=EDGE_CURVE('',#3710,#3706,#2118,.T.);
#4379=EDGE_CURVE('',#3711,#3709,#2119,.T.);
#4380=EDGE_CURVE('',#3710,#3711,#2120,.T.);
#4381=EDGE_CURVE('',#3712,#3710,#2121,.T.);
#4382=EDGE_CURVE('',#3713,#3711,#2122,.T.);
#4383=EDGE_CURVE('',#3712,#3713,#2123,.T.);
#4384=EDGE_CURVE('',#3707,#3712,#2124,.T.);
#4385=EDGE_CURVE('',#3708,#3713,#2125,.T.);
#4386=EDGE_CURVE('',#3714,#3715,#2126,.T.);
#4387=EDGE_CURVE('',#3716,#3715,#3418,.T.);
#4388=EDGE_CURVE('',#3717,#3716,#2127,.T.);
#4389=EDGE_CURVE('',#3714,#3717,#3419,.T.);
#4390=EDGE_CURVE('',#3714,#3715,#2128,.T.);
#4391=EDGE_CURVE('',#3717,#3714,#3420,.T.);
#4392=EDGE_CURVE('',#3717,#3716,#2129,.T.);
#4393=EDGE_CURVE('',#3715,#3716,#3421,.T.);
#4394=EDGE_CURVE('',#3718,#3718,#3422,.T.);
#4395=EDGE_CURVE('',#3719,#3720,#2130,.T.);
#4396=EDGE_CURVE('',#3721,#3720,#3423,.T.);
#4397=EDGE_CURVE('',#3722,#3721,#2131,.T.);
#4398=EDGE_CURVE('',#3719,#3722,#3424,.T.);
#4399=EDGE_CURVE('',#3719,#3720,#2132,.T.);
#4400=EDGE_CURVE('',#3722,#3719,#3425,.T.);
#4401=EDGE_CURVE('',#3722,#3721,#2133,.T.);
#4402=EDGE_CURVE('',#3720,#3721,#3426,.T.);
#4403=EDGE_CURVE('',#3723,#3723,#3427,.T.);
#4404=EDGE_CURVE('',#3720,#3724,#2134,.T.);
#4405=EDGE_CURVE('',#3724,#3725,#2135,.T.);
#4406=EDGE_CURVE('',#3725,#3721,#2136,.T.);
#4407=EDGE_CURVE('',#3715,#3720,#2137,.T.);
#4408=EDGE_CURVE('',#3721,#3716,#2138,.T.);
#4409=EDGE_CURVE('',#3716,#3726,#2139,.T.);
#4410=EDGE_CURVE('',#3726,#3727,#2140,.T.);
#4411=EDGE_CURVE('',#3727,#3715,#2141,.T.);
#4412=EDGE_CURVE('',#3728,#3728,#3428,.T.);
#4413=EDGE_CURVE('',#3728,#3718,#2142,.T.);
#4414=EDGE_CURVE('',#3729,#3729,#3429,.T.);
#4415=EDGE_CURVE('',#3729,#3723,#2143,.T.);
#4416=EDGE_CURVE('',#3730,#3731,#2144,.T.);
#4417=EDGE_CURVE('',#3731,#3725,#2145,.T.);
#4418=EDGE_CURVE('',#3730,#3724,#2146,.T.);
#4419=EDGE_CURVE('',#3732,#3730,#2147,.T.);
#4420=EDGE_CURVE('',#3732,#3727,#2148,.T.);
#4421=EDGE_CURVE('',#3733,#3732,#2149,.T.);
#4422=EDGE_CURVE('',#3733,#3726,#2150,.T.);
#4423=EDGE_CURVE('',#3731,#3733,#2151,.T.);
#4424=EDGE_CURVE('',#3734,#3735,#2152,.T.);
#4425=EDGE_CURVE('',#3735,#3736,#2153,.T.);
#4426=EDGE_CURVE('',#3737,#3736,#2154,.T.);
#4427=EDGE_CURVE('',#3734,#3737,#2155,.T.);
#4428=EDGE_CURVE('',#3738,#3734,#2156,.T.);
#4429=EDGE_CURVE('',#3739,#3737,#2157,.T.);
#4430=EDGE_CURVE('',#3738,#3739,#2158,.T.);
#4431=EDGE_CURVE('',#3740,#3738,#2159,.T.);
#4432=EDGE_CURVE('',#3741,#3739,#2160,.T.);
#4433=EDGE_CURVE('',#3740,#3741,#2161,.T.);
#4434=EDGE_CURVE('',#3735,#3740,#2162,.T.);
#4435=EDGE_CURVE('',#3736,#3741,#2163,.T.);
#4436=EDGE_CURVE('',#3742,#3743,#2164,.T.);
#4437=EDGE_CURVE('',#3742,#3744,#2165,.T.);
#4438=EDGE_CURVE('',#3745,#3744,#2166,.T.);
#4439=EDGE_CURVE('',#3743,#3745,#2167,.T.);
#4440=EDGE_CURVE('',#3746,#3742,#2168,.T.);
#4441=EDGE_CURVE('',#3746,#3747,#2169,.T.);
#4442=EDGE_CURVE('',#3744,#3747,#2170,.T.);
#4443=EDGE_CURVE('',#3748,#3746,#2171,.T.);
#4444=EDGE_CURVE('',#3748,#3749,#2172,.T.);
#4445=EDGE_CURVE('',#3747,#3749,#2173,.T.);
#4446=EDGE_CURVE('',#3750,#3748,#2174,.T.);
#4447=EDGE_CURVE('',#3750,#3751,#2175,.T.);
#4448=EDGE_CURVE('',#3749,#3751,#2176,.T.);
#4449=EDGE_CURVE('',#3752,#3750,#2177,.T.);
#4450=EDGE_CURVE('',#3752,#3753,#2178,.T.);
#4451=EDGE_CURVE('',#3751,#3753,#2179,.T.);
#4452=EDGE_CURVE('',#3754,#3752,#2180,.T.);
#4453=EDGE_CURVE('',#3754,#3755,#2181,.T.);
#4454=EDGE_CURVE('',#3753,#3755,#2182,.T.);
#4455=EDGE_CURVE('',#3756,#3754,#2183,.T.);
#4456=EDGE_CURVE('',#3756,#3757,#2184,.T.);
#4457=EDGE_CURVE('',#3755,#3757,#2185,.T.);
#4458=EDGE_CURVE('',#3758,#3756,#2186,.T.);
#4459=EDGE_CURVE('',#3758,#3759,#2187,.T.);
#4460=EDGE_CURVE('',#3757,#3759,#2188,.T.);
#4461=EDGE_CURVE('',#3760,#3758,#2189,.T.);
#4462=EDGE_CURVE('',#3761,#3760,#2190,.T.);
#4463=EDGE_CURVE('',#3759,#3761,#2191,.T.);
#4464=EDGE_CURVE('',#3762,#3763,#2192,.T.);
#4465=EDGE_CURVE('',#3762,#3764,#2193,.T.);
#4466=EDGE_CURVE('',#3765,#3764,#2194,.T.);
#4467=EDGE_CURVE('',#3763,#3765,#2195,.T.);
#4468=EDGE_CURVE('',#3766,#3762,#2196,.T.);
#4469=EDGE_CURVE('',#3766,#3767,#2197,.T.);
#4470=EDGE_CURVE('',#3764,#3767,#2198,.T.);
#4471=EDGE_CURVE('',#3768,#3766,#2199,.T.);
#4472=EDGE_CURVE('',#3768,#3769,#2200,.T.);
#4473=EDGE_CURVE('',#3767,#3769,#2201,.T.);
#4474=EDGE_CURVE('',#3770,#3768,#2202,.T.);
#4475=EDGE_CURVE('',#3770,#3771,#2203,.T.);
#4476=EDGE_CURVE('',#3769,#3771,#2204,.T.);
#4477=EDGE_CURVE('',#3772,#3770,#2205,.T.);
#4478=EDGE_CURVE('',#3772,#3773,#2206,.T.);
#4479=EDGE_CURVE('',#3771,#3773,#2207,.T.);
#4480=EDGE_CURVE('',#3774,#3772,#2208,.T.);
#4481=EDGE_CURVE('',#3774,#3775,#2209,.T.);
#4482=EDGE_CURVE('',#3773,#3775,#2210,.T.);
#4483=EDGE_CURVE('',#3776,#3774,#2211,.T.);
#4484=EDGE_CURVE('',#3776,#3777,#2212,.T.);
#4485=EDGE_CURVE('',#3775,#3777,#2213,.T.);
#4486=EDGE_CURVE('',#3778,#3776,#2214,.T.);
#4487=EDGE_CURVE('',#3778,#3779,#2215,.T.);
#4488=EDGE_CURVE('',#3777,#3779,#2216,.T.);
#4489=EDGE_CURVE('',#3780,#3778,#2217,.T.);
#4490=EDGE_CURVE('',#3781,#3780,#2218,.T.);
#4491=EDGE_CURVE('',#3779,#3781,#2219,.T.);
#4492=EDGE_CURVE('',#3782,#3783,#2220,.T.);
#4493=EDGE_CURVE('',#3782,#3784,#2221,.T.);
#4494=EDGE_CURVE('',#3785,#3784,#2222,.T.);
#4495=EDGE_CURVE('',#3783,#3785,#2223,.T.);
#4496=EDGE_CURVE('',#3786,#3782,#2224,.T.);
#4497=EDGE_CURVE('',#3786,#3787,#2225,.T.);
#4498=EDGE_CURVE('',#3784,#3787,#2226,.T.);
#4499=EDGE_CURVE('',#3788,#3786,#2227,.T.);
#4500=EDGE_CURVE('',#3788,#3789,#2228,.T.);
#4501=EDGE_CURVE('',#3787,#3789,#2229,.T.);
#4502=EDGE_CURVE('',#3790,#3788,#2230,.T.);
#4503=EDGE_CURVE('',#3790,#3791,#2231,.T.);
#4504=EDGE_CURVE('',#3789,#3791,#2232,.T.);
#4505=EDGE_CURVE('',#3792,#3790,#2233,.T.);
#4506=EDGE_CURVE('',#3792,#3793,#2234,.T.);
#4507=EDGE_CURVE('',#3791,#3793,#2235,.T.);
#4508=EDGE_CURVE('',#3794,#3792,#2236,.T.);
#4509=EDGE_CURVE('',#3794,#3795,#2237,.T.);
#4510=EDGE_CURVE('',#3793,#3795,#2238,.T.);
#4511=EDGE_CURVE('',#3796,#3794,#2239,.T.);
#4512=EDGE_CURVE('',#3796,#3797,#2240,.T.);
#4513=EDGE_CURVE('',#3795,#3797,#2241,.T.);
#4514=EDGE_CURVE('',#3798,#3796,#2242,.T.);
#4515=EDGE_CURVE('',#3798,#3799,#2243,.T.);
#4516=EDGE_CURVE('',#3797,#3799,#2244,.T.);
#4517=EDGE_CURVE('',#3800,#3798,#2245,.T.);
#4518=EDGE_CURVE('',#3801,#3800,#2246,.T.);
#4519=EDGE_CURVE('',#3799,#3801,#2247,.T.);
#4520=EDGE_CURVE('',#3802,#3803,#2248,.T.);
#4521=EDGE_CURVE('',#3802,#3804,#2249,.T.);
#4522=EDGE_CURVE('',#3805,#3804,#2250,.T.);
#4523=EDGE_CURVE('',#3803,#3805,#2251,.T.);
#4524=EDGE_CURVE('',#3806,#3802,#2252,.T.);
#4525=EDGE_CURVE('',#3806,#3807,#2253,.T.);
#4526=EDGE_CURVE('',#3804,#3807,#2254,.T.);
#4527=EDGE_CURVE('',#3808,#3806,#2255,.T.);
#4528=EDGE_CURVE('',#3808,#3809,#2256,.T.);
#4529=EDGE_CURVE('',#3807,#3809,#2257,.T.);
#4530=EDGE_CURVE('',#3810,#3808,#2258,.T.);
#4531=EDGE_CURVE('',#3810,#3811,#2259,.T.);
#4532=EDGE_CURVE('',#3809,#3811,#2260,.T.);
#4533=EDGE_CURVE('',#3812,#3810,#2261,.T.);
#4534=EDGE_CURVE('',#3812,#3813,#2262,.T.);
#4535=EDGE_CURVE('',#3811,#3813,#2263,.T.);
#4536=EDGE_CURVE('',#3814,#3812,#2264,.T.);
#4537=EDGE_CURVE('',#3814,#3815,#2265,.T.);
#4538=EDGE_CURVE('',#3813,#3815,#2266,.T.);
#4539=EDGE_CURVE('',#3816,#3814,#2267,.T.);
#4540=EDGE_CURVE('',#3816,#3817,#2268,.T.);
#4541=EDGE_CURVE('',#3815,#3817,#2269,.T.);
#4542=EDGE_CURVE('',#3818,#3816,#2270,.T.);
#4543=EDGE_CURVE('',#3818,#3819,#2271,.T.);
#4544=EDGE_CURVE('',#3817,#3819,#2272,.T.);
#4545=EDGE_CURVE('',#3820,#3818,#2273,.T.);
#4546=EDGE_CURVE('',#3821,#3820,#2274,.T.);
#4547=EDGE_CURVE('',#3819,#3821,#2275,.T.);
#4548=EDGE_CURVE('',#3822,#3822,#3430,.T.);
#4549=EDGE_CURVE('',#3822,#3823,#2276,.T.);
#4550=EDGE_CURVE('',#3823,#3823,#3431,.T.);
#4551=EDGE_CURVE('',#3760,#3824,#2277,.T.);
#4552=EDGE_CURVE('',#3824,#3825,#2278,.T.);
#4553=EDGE_CURVE('',#3761,#3825,#2279,.T.);
#4554=EDGE_CURVE('',#3826,#3745,#2280,.T.);
#4555=EDGE_CURVE('',#3827,#3826,#2281,.T.);
#4556=EDGE_CURVE('',#3827,#3743,#2282,.T.);
#4557=EDGE_CURVE('',#3780,#3827,#2283,.T.);
#4558=EDGE_CURVE('',#3781,#3826,#2284,.T.);
#4559=EDGE_CURVE('',#3828,#3765,#2285,.T.);
#4560=EDGE_CURVE('',#3829,#3828,#2286,.T.);
#4561=EDGE_CURVE('',#3829,#3763,#2287,.T.);
#4562=EDGE_CURVE('',#3800,#3829,#2288,.T.);
#4563=EDGE_CURVE('',#3801,#3828,#2289,.T.);
#4564=EDGE_CURVE('',#3830,#3785,#2290,.T.);
#4565=EDGE_CURVE('',#3831,#3830,#2291,.T.);
#4566=EDGE_CURVE('',#3831,#3783,#2292,.T.);
#4567=EDGE_CURVE('',#3820,#3831,#2293,.T.);
#4568=EDGE_CURVE('',#3821,#3830,#2294,.T.);
#4569=EDGE_CURVE('',#3825,#3805,#2295,.T.);
#4570=EDGE_CURVE('',#3824,#3803,#2296,.T.);
#4571=EDGE_CURVE('',#3832,#3832,#3432,.T.);
#4572=EDGE_CURVE('',#3832,#3833,#2297,.T.);
#4573=EDGE_CURVE('',#3833,#3833,#3433,.T.);
#4574=EDGE_CURVE('',#3834,#3834,#3434,.T.);
#4575=EDGE_CURVE('',#3835,#3835,#3435,.T.);
#4576=EDGE_CURVE('',#3835,#3836,#2298,.T.);
#4577=EDGE_CURVE('',#3836,#3836,#3436,.T.);
#4578=EDGE_CURVE('',#3837,#3837,#3437,.T.);
#4579=EDGE_CURVE('',#3838,#3838,#3438,.T.);
#4580=EDGE_CURVE('',#3838,#3839,#2299,.T.);
#4581=EDGE_CURVE('',#3839,#3839,#3439,.T.);
#4582=EDGE_CURVE('',#3840,#3840,#3440,.T.);
#4583=EDGE_CURVE('',#3841,#3841,#3441,.T.);
#4584=EDGE_CURVE('',#3841,#3842,#2300,.T.);
#4585=EDGE_CURVE('',#3842,#3842,#3442,.T.);
#4586=EDGE_CURVE('',#3843,#3843,#3443,.T.);
#4587=EDGE_CURVE('',#3844,#3844,#3444,.T.);
#4588=EDGE_CURVE('',#3844,#3834,#2301,.T.);
#4589=EDGE_CURVE('',#3845,#3845,#3445,.T.);
#4590=EDGE_CURVE('',#3845,#3837,#2302,.T.);
#4591=EDGE_CURVE('',#3846,#3846,#3446,.T.);
#4592=EDGE_CURVE('',#3846,#3840,#2303,.T.);
#4593=EDGE_CURVE('',#3847,#3847,#3447,.T.);
#4594=EDGE_CURVE('',#3847,#3843,#2304,.T.);
#4595=EDGE_CURVE('',#3848,#3849,#2305,.T.);
#4596=EDGE_CURVE('',#3849,#3850,#2306,.T.);
#4597=EDGE_CURVE('',#3851,#3850,#2307,.T.);
#4598=EDGE_CURVE('',#3848,#3851,#2308,.T.);
#4599=EDGE_CURVE('',#3852,#3848,#2309,.T.);
#4600=EDGE_CURVE('',#3853,#3851,#2310,.T.);
#4601=EDGE_CURVE('',#3852,#3853,#2311,.T.);
#4602=EDGE_CURVE('',#3854,#3852,#2312,.T.);
#4603=EDGE_CURVE('',#3855,#3853,#2313,.T.);
#4604=EDGE_CURVE('',#3854,#3855,#2314,.T.);
#4605=EDGE_CURVE('',#3856,#3854,#2315,.T.);
#4606=EDGE_CURVE('',#3857,#3855,#2316,.T.);
#4607=EDGE_CURVE('',#3856,#3857,#2317,.T.);
#4608=EDGE_CURVE('',#3858,#3856,#2318,.T.);
#4609=EDGE_CURVE('',#3859,#3857,#2319,.T.);
#4610=EDGE_CURVE('',#3858,#3859,#2320,.T.);
#4611=EDGE_CURVE('',#3860,#3858,#2321,.T.);
#4612=EDGE_CURVE('',#3861,#3859,#2322,.T.);
#4613=EDGE_CURVE('',#3860,#3861,#2323,.T.);
#4614=EDGE_CURVE('',#3862,#3860,#2324,.T.);
#4615=EDGE_CURVE('',#3863,#3861,#2325,.T.);
#4616=EDGE_CURVE('',#3862,#3863,#2326,.T.);
#4617=EDGE_CURVE('',#3864,#3862,#2327,.T.);
#4618=EDGE_CURVE('',#3865,#3863,#2328,.T.);
#4619=EDGE_CURVE('',#3864,#3865,#2329,.T.);
#4620=EDGE_CURVE('',#3866,#3864,#2330,.T.);
#4621=EDGE_CURVE('',#3867,#3865,#2331,.T.);
#4622=EDGE_CURVE('',#3866,#3867,#2332,.T.);
#4623=EDGE_CURVE('',#3868,#3866,#2333,.T.);
#4624=EDGE_CURVE('',#3869,#3867,#2334,.T.);
#4625=EDGE_CURVE('',#3868,#3869,#2335,.T.);
#4626=EDGE_CURVE('',#3870,#3868,#2336,.T.);
#4627=EDGE_CURVE('',#3871,#3869,#2337,.T.);
#4628=EDGE_CURVE('',#3870,#3871,#2338,.T.);
#4629=EDGE_CURVE('',#3849,#3870,#2339,.T.);
#4630=EDGE_CURVE('',#3850,#3871,#2340,.T.);
#4631=EDGE_CURVE('',#3872,#3872,#3448,.T.);
#4632=EDGE_CURVE('',#3873,#3873,#3449,.T.);
#4633=EDGE_CURVE('',#3873,#3872,#2341,.T.);
#4634=EDGE_CURVE('',#3874,#3874,#3450,.T.);
#4635=EDGE_CURVE('',#3874,#3873,#2342,.T.);
#4636=EDGE_CURVE('',#3875,#3875,#3451,.T.);
#4637=EDGE_CURVE('',#3875,#3874,#2343,.T.);
#4638=EDGE_CURVE('',#3876,#3876,#3452,.T.);
#4639=EDGE_CURVE('',#3877,#3877,#3453,.F.);
#4640=EDGE_CURVE('',#3877,#3876,#2344,.T.);
#4641=EDGE_CURVE('',#3878,#3878,#3454,.F.);
#4642=EDGE_CURVE('',#3878,#3877,#2345,.T.);
#4643=EDGE_CURVE('',#3879,#3879,#3455,.T.);
#4644=EDGE_CURVE('',#3879,#3878,#2346,.T.);
#4645=EDGE_CURVE('',#3880,#3881,#2347,.T.);
#4646=EDGE_CURVE('',#3881,#3882,#2348,.T.);
#4647=EDGE_CURVE('',#3882,#3883,#2349,.T.);
#4648=EDGE_CURVE('',#3880,#3883,#2350,.T.);
#4649=EDGE_CURVE('',#3881,#3884,#2351,.T.);
#4650=EDGE_CURVE('',#3884,#3885,#2352,.T.);
#4651=EDGE_CURVE('',#3885,#3882,#2353,.T.);
#4652=EDGE_CURVE('',#3884,#3886,#2354,.T.);
#4653=EDGE_CURVE('',#3886,#3887,#2355,.T.);
#4654=EDGE_CURVE('',#3887,#3885,#2356,.T.);
#4655=EDGE_CURVE('',#3886,#3888,#2357,.T.);
#4656=EDGE_CURVE('',#3888,#3889,#2358,.T.);
#4657=EDGE_CURVE('',#3889,#3887,#2359,.T.);
#4658=EDGE_CURVE('',#3888,#3890,#2360,.T.);
#4659=EDGE_CURVE('',#3890,#3891,#2361,.T.);
#4660=EDGE_CURVE('',#3891,#3889,#2362,.T.);
#4661=EDGE_CURVE('',#3890,#3880,#2363,.T.);
#4662=EDGE_CURVE('',#3883,#3891,#2364,.T.);
#4663=EDGE_CURVE('',#3892,#3893,#2365,.T.);
#4664=EDGE_CURVE('',#3894,#3892,#2366,.T.);
#4665=EDGE_CURVE('',#3895,#3894,#2367,.T.);
#4666=EDGE_CURVE('',#3893,#3895,#2368,.T.);
#4667=EDGE_CURVE('',#3894,#3896,#2369,.T.);
#4668=EDGE_CURVE('',#3897,#3896,#2370,.T.);
#4669=EDGE_CURVE('',#3895,#3897,#2371,.T.);
#4670=EDGE_CURVE('',#3896,#3898,#2372,.T.);
#4671=EDGE_CURVE('',#3898,#3899,#2373,.T.);
#4672=EDGE_CURVE('',#3899,#3897,#2374,.T.);
#4673=EDGE_CURVE('',#3900,#3900,#3456,.T.);
#4674=EDGE_CURVE('',#3901,#3892,#2375,.T.);
#4675=EDGE_CURVE('',#3902,#3901,#2376,.T.);
#4676=EDGE_CURVE('',#3902,#3903,#2377,.T.);
#4677=EDGE_CURVE('',#3904,#3903,#2378,.T.);
#4678=EDGE_CURVE('',#3904,#3905,#2379,.T.);
#4679=EDGE_CURVE('',#3905,#3906,#2380,.T.);
#4680=EDGE_CURVE('',#3906,#3898,#2381,.T.);
#4681=EDGE_CURVE('',#3906,#3907,#2382,.T.);
#4682=EDGE_CURVE('',#3907,#3899,#2383,.T.);
#4683=EDGE_CURVE('',#3908,#3905,#2384,.T.);
#4684=EDGE_CURVE('',#3907,#3908,#2385,.T.);
#4685=EDGE_CURVE('',#3909,#3908,#2386,.T.);
#4686=EDGE_CURVE('',#3910,#3909,#2387,.T.);
#4687=EDGE_CURVE('',#3910,#3911,#2388,.T.);
#4688=EDGE_CURVE('',#3912,#3911,#2389,.T.);
#4689=EDGE_CURVE('',#3912,#3893,#2390,.T.);
#4690=EDGE_CURVE('',#3909,#3904,#2391,.T.);
#4691=EDGE_CURVE('',#3903,#3913,#2392,.T.);
#4692=EDGE_CURVE('',#3913,#3914,#491,.T.);
#4693=EDGE_CURVE('',#3914,#3910,#2393,.T.);
#4694=EDGE_CURVE('',#3915,#3913,#3457,.F.);
#4695=EDGE_CURVE('',#3915,#3900,#2394,.T.);
#4696=EDGE_CURVE('',#3916,#3915,#3458,.F.);
#4697=EDGE_CURVE('',#3917,#3916,#492,.T.);
#4698=EDGE_CURVE('',#3914,#3917,#3459,.F.);
#4699=EDGE_CURVE('',#3916,#3902,#2395,.T.);
#4700=EDGE_CURVE('',#3911,#3917,#2396,.T.);
#4701=EDGE_CURVE('',#3901,#3912,#2397,.T.);
#4702=EDGE_CURVE('',#3918,#3919,#2398,.T.);
#4703=EDGE_CURVE('',#3919,#3920,#2399,.T.);
#4704=EDGE_CURVE('',#3920,#3921,#2400,.T.);
#4705=EDGE_CURVE('',#3918,#3921,#2401,.T.);
#4706=EDGE_CURVE('',#3919,#3922,#2402,.T.);
#4707=EDGE_CURVE('',#3922,#3923,#2403,.T.);
#4708=EDGE_CURVE('',#3923,#3920,#2404,.T.);
#4709=EDGE_CURVE('',#3922,#3924,#2405,.T.);
#4710=EDGE_CURVE('',#3924,#3925,#2406,.T.);
#4711=EDGE_CURVE('',#3925,#3923,#2407,.T.);
#4712=EDGE_CURVE('',#3924,#3926,#2408,.T.);
#4713=EDGE_CURVE('',#3926,#3927,#2409,.T.);
#4714=EDGE_CURVE('',#3927,#3925,#2410,.T.);
#4715=EDGE_CURVE('',#3926,#3928,#2411,.T.);
#4716=EDGE_CURVE('',#3928,#3929,#2412,.T.);
#4717=EDGE_CURVE('',#3929,#3927,#2413,.T.);
#4718=EDGE_CURVE('',#3928,#3918,#2414,.T.);
#4719=EDGE_CURVE('',#3921,#3929,#2415,.T.);
#4720=EDGE_CURVE('',#3930,#3930,#3460,.T.);
#4721=EDGE_CURVE('',#3931,#3931,#3461,.T.);
#4722=EDGE_CURVE('',#3932,#3932,#3462,.T.);
#4723=EDGE_CURVE('',#3932,#3931,#2416,.T.);
#4724=EDGE_CURVE('',#3933,#3933,#3463,.T.);
#4725=EDGE_CURVE('',#3933,#3932,#2417,.T.);
#4726=EDGE_CURVE('',#3934,#3934,#3464,.T.);
#4727=EDGE_CURVE('',#3934,#3933,#2418,.T.);
#4728=EDGE_CURVE('',#3935,#3935,#3465,.T.);
#4729=EDGE_CURVE('',#3936,#3936,#3466,.F.);
#4730=EDGE_CURVE('',#3936,#3935,#2419,.T.);
#4731=EDGE_CURVE('',#3930,#3936,#2420,.T.);
#4732=EDGE_CURVE('',#3937,#3937,#3467,.T.);
#4733=EDGE_CURVE('',#3937,#3938,#2421,.T.);
#4734=EDGE_CURVE('',#3938,#3938,#3468,.T.);
#4735=EDGE_CURVE('',#3939,#3939,#3469,.T.);
#4736=EDGE_CURVE('',#3939,#3940,#2422,.T.);
#4737=EDGE_CURVE('',#3940,#3940,#3470,.T.);
#4738=EDGE_CURVE('',#3941,#3941,#3471,.T.);
#4739=EDGE_CURVE('',#3941,#3942,#2423,.T.);
#4740=EDGE_CURVE('',#3942,#3942,#3472,.T.);
#4741=EDGE_CURVE('',#3943,#3943,#3473,.T.);
#4742=EDGE_CURVE('',#3943,#3944,#2424,.T.);
#4743=EDGE_CURVE('',#3944,#3944,#3474,.T.);
#4744=EDGE_CURVE('',#3945,#3945,#3475,.T.);
#4745=EDGE_CURVE('',#3945,#3946,#2425,.T.);
#4746=EDGE_CURVE('',#3946,#3946,#3476,.T.);
#4747=EDGE_CURVE('',#3947,#3947,#3477,.T.);
#4748=EDGE_CURVE('',#3947,#3948,#2426,.T.);
#4749=EDGE_CURVE('',#3948,#3948,#3478,.T.);
#4750=EDGE_CURVE('',#3949,#3949,#3479,.T.);
#4751=EDGE_CURVE('',#3949,#3950,#2427,.T.);
#4752=EDGE_CURVE('',#3950,#3950,#3480,.T.);
#4753=EDGE_CURVE('',#3951,#3951,#3481,.T.);
#4754=EDGE_CURVE('',#3951,#3952,#2428,.T.);
#4755=EDGE_CURVE('',#3952,#3952,#3482,.T.);
#4756=EDGE_CURVE('',#3953,#3953,#3483,.T.);
#4757=EDGE_CURVE('',#3953,#3954,#2429,.T.);
#4758=EDGE_CURVE('',#3954,#3954,#3484,.T.);
#4759=EDGE_CURVE('',#3955,#3955,#3485,.T.);
#4760=EDGE_CURVE('',#3955,#3956,#2430,.T.);
#4761=EDGE_CURVE('',#3956,#3956,#3486,.T.);
#4762=EDGE_CURVE('',#3957,#3957,#3487,.T.);
#4763=EDGE_CURVE('',#3957,#3958,#2431,.T.);
#4764=EDGE_CURVE('',#3958,#3958,#3488,.T.);
#4765=EDGE_CURVE('',#3959,#3959,#3489,.T.);
#4766=EDGE_CURVE('',#3959,#3960,#2432,.T.);
#4767=EDGE_CURVE('',#3960,#3960,#3490,.T.);
#4768=EDGE_CURVE('',#3961,#3961,#3491,.T.);
#4769=EDGE_CURVE('',#3961,#3962,#2433,.T.);
#4770=EDGE_CURVE('',#3962,#3962,#3492,.T.);
#4771=EDGE_CURVE('',#3963,#3963,#3493,.T.);
#4772=EDGE_CURVE('',#3963,#3964,#2434,.T.);
#4773=EDGE_CURVE('',#3964,#3964,#3494,.T.);
#4774=EDGE_CURVE('',#3965,#3965,#3495,.T.);
#4775=EDGE_CURVE('',#3965,#3966,#2435,.T.);
#4776=EDGE_CURVE('',#3966,#3966,#3496,.T.);
#4777=EDGE_CURVE('',#3967,#3967,#3497,.T.);
#4778=EDGE_CURVE('',#3967,#3968,#2436,.T.);
#4779=EDGE_CURVE('',#3968,#3968,#3498,.T.);
#4780=EDGE_CURVE('',#3969,#3969,#3499,.T.);
#4781=EDGE_CURVE('',#3969,#3970,#2437,.T.);
#4782=EDGE_CURVE('',#3970,#3970,#3500,.T.);
#4783=EDGE_CURVE('',#3971,#3971,#3501,.T.);
#4784=EDGE_CURVE('',#3971,#3972,#2438,.T.);
#4785=EDGE_CURVE('',#3972,#3972,#3502,.T.);
#4786=EDGE_CURVE('',#3973,#3973,#3503,.T.);
#4787=EDGE_CURVE('',#3973,#3974,#2439,.T.);
#4788=EDGE_CURVE('',#3974,#3974,#3504,.T.);
#4789=EDGE_CURVE('',#3975,#3976,#2440,.T.);
#4790=EDGE_CURVE('',#3976,#3977,#2441,.T.);
#4791=EDGE_CURVE('',#3978,#3977,#2442,.T.);
#4792=EDGE_CURVE('',#3975,#3978,#2443,.T.);
#4793=EDGE_CURVE('',#3979,#3975,#2444,.T.);
#4794=EDGE_CURVE('',#3980,#3978,#2445,.T.);
#4795=EDGE_CURVE('',#3979,#3980,#2446,.T.);
#4796=EDGE_CURVE('',#3981,#3979,#2447,.T.);
#4797=EDGE_CURVE('',#3982,#3980,#2448,.T.);
#4798=EDGE_CURVE('',#3981,#3982,#2449,.T.);
#4799=EDGE_CURVE('',#3976,#3981,#2450,.T.);
#4800=EDGE_CURVE('',#3977,#3982,#2451,.T.);
#4801=EDGE_CURVE('',#3983,#3983,#3505,.T.);
#4802=EDGE_CURVE('',#3983,#3984,#2452,.T.);
#4803=EDGE_CURVE('',#3984,#3984,#3506,.T.);
#4804=EDGE_CURVE('',#3985,#3985,#3507,.T.);
#4805=EDGE_CURVE('',#3985,#3986,#2453,.T.);
#4806=EDGE_CURVE('',#3986,#3986,#3508,.T.);
#4807=EDGE_CURVE('',#3987,#3987,#3509,.T.);
#4808=EDGE_CURVE('',#3987,#3988,#2454,.T.);
#4809=EDGE_CURVE('',#3988,#3988,#3510,.T.);
#4810=EDGE_CURVE('',#3989,#3989,#3511,.T.);
#4811=EDGE_CURVE('',#3989,#3990,#2455,.T.);
#4812=EDGE_CURVE('',#3990,#3990,#3512,.T.);
#4813=EDGE_CURVE('',#3991,#3992,#2456,.T.);
#4814=EDGE_CURVE('',#3992,#3993,#2457,.T.);
#4815=EDGE_CURVE('',#3994,#3993,#2458,.T.);
#4816=EDGE_CURVE('',#3991,#3994,#2459,.T.);
#4817=EDGE_CURVE('',#3995,#3991,#2460,.T.);
#4818=EDGE_CURVE('',#3996,#3994,#2461,.T.);
#4819=EDGE_CURVE('',#3995,#3996,#2462,.T.);
#4820=EDGE_CURVE('',#3997,#3995,#2463,.T.);
#4821=EDGE_CURVE('',#3998,#3996,#2464,.T.);
#4822=EDGE_CURVE('',#3997,#3998,#2465,.T.);
#4823=EDGE_CURVE('',#3999,#3997,#2466,.T.);
#4824=EDGE_CURVE('',#4000,#3998,#2467,.T.);
#4825=EDGE_CURVE('',#3999,#4000,#2468,.T.);
#4826=EDGE_CURVE('',#4001,#3999,#2469,.T.);
#4827=EDGE_CURVE('',#4002,#4000,#2470,.T.);
#4828=EDGE_CURVE('',#4001,#4002,#2471,.T.);
#4829=EDGE_CURVE('',#3992,#4001,#2472,.T.);
#4830=EDGE_CURVE('',#3993,#4002,#2473,.T.);
#4831=EDGE_CURVE('',#4003,#4004,#2474,.T.);
#4832=EDGE_CURVE('',#4003,#4004,#3513,.T.);
#4833=EDGE_CURVE('',#4005,#4003,#2475,.T.);
#4834=EDGE_CURVE('',#4006,#4005,#3514,.T.);
#4835=EDGE_CURVE('',#4006,#4007,#2476,.T.);
#4836=EDGE_CURVE('',#4007,#4007,#3515,.T.);
#4837=EDGE_CURVE('',#4008,#4006,#3516,.T.);
#4838=EDGE_CURVE('',#4004,#4008,#2477,.T.);
#4839=EDGE_CURVE('',#4009,#4010,#2478,.T.);
#4840=EDGE_CURVE('',#4009,#4010,#3517,.T.);
#4841=EDGE_CURVE('',#4011,#4009,#2479,.T.);
#4842=EDGE_CURVE('',#4012,#4011,#3518,.T.);
#4843=EDGE_CURVE('',#4012,#4013,#2480,.T.);
#4844=EDGE_CURVE('',#4013,#4013,#3519,.T.);
#4845=EDGE_CURVE('',#4014,#4012,#3520,.T.);
#4846=EDGE_CURVE('',#4010,#4014,#2481,.T.);
#4847=EDGE_CURVE('',#4015,#4016,#2482,.T.);
#4848=EDGE_CURVE('',#4015,#4016,#3521,.T.);
#4849=EDGE_CURVE('',#4017,#4015,#2483,.T.);
#4850=EDGE_CURVE('',#4018,#4017,#3522,.T.);
#4851=EDGE_CURVE('',#4018,#4019,#2484,.T.);
#4852=EDGE_CURVE('',#4019,#4019,#3523,.T.);
#4853=EDGE_CURVE('',#4020,#4018,#3524,.T.);
#4854=EDGE_CURVE('',#4016,#4020,#2485,.T.);
#4855=EDGE_CURVE('',#4021,#4022,#2486,.T.);
#4856=EDGE_CURVE('',#4021,#4022,#3525,.T.);
#4857=EDGE_CURVE('',#4023,#4021,#2487,.T.);
#4858=EDGE_CURVE('',#4024,#4023,#3526,.T.);
#4859=EDGE_CURVE('',#4024,#4025,#2488,.T.);
#4860=EDGE_CURVE('',#4025,#4025,#3527,.T.);
#4861=EDGE_CURVE('',#4026,#4024,#3528,.T.);
#4862=EDGE_CURVE('',#4022,#4026,#2489,.T.);
#4863=EDGE_CURVE('',#4008,#4017,#2490,.T.);
#4864=EDGE_CURVE('',#4020,#4027,#2491,.T.);
#4865=EDGE_CURVE('',#4028,#4027,#2492,.T.);
#4866=EDGE_CURVE('',#4028,#4029,#2493,.T.);
#4867=EDGE_CURVE('',#4030,#4029,#2494,.T.);
#4868=EDGE_CURVE('',#4030,#4005,#2495,.T.);
#4869=EDGE_CURVE('',#4014,#4023,#2496,.T.);
#4870=EDGE_CURVE('',#4026,#4031,#2497,.T.);
#4871=EDGE_CURVE('',#4032,#4031,#2498,.T.);
#4872=EDGE_CURVE('',#4033,#4032,#2499,.T.);
#4873=EDGE_CURVE('',#4034,#4033,#2500,.T.);
#4874=EDGE_CURVE('',#4034,#4011,#2501,.T.);
#4875=EDGE_CURVE('',#4027,#4035,#2502,.T.);
#4876=EDGE_CURVE('',#4035,#4036,#2503,.T.);
#4877=EDGE_CURVE('',#4036,#4037,#2504,.T.);
#4878=EDGE_CURVE('',#4037,#4038,#2505,.T.);
#4879=EDGE_CURVE('',#4038,#4034,#2506,.T.);
#4880=EDGE_CURVE('',#4033,#4039,#2507,.T.);
#4881=EDGE_CURVE('',#4039,#4040,#2508,.T.);
#4882=EDGE_CURVE('',#4040,#4041,#2509,.T.);
#4883=EDGE_CURVE('',#4041,#4042,#2510,.T.);
#4884=EDGE_CURVE('',#4042,#4028,#2511,.T.);
#4885=EDGE_CURVE('',#4043,#4030,#2512,.T.);
#4886=EDGE_CURVE('',#4035,#4043,#2513,.T.);
#4887=EDGE_CURVE('',#4044,#4043,#2514,.T.);
#4888=EDGE_CURVE('',#4036,#4044,#2515,.T.);
#4889=EDGE_CURVE('',#4045,#4044,#2516,.T.);
#4890=EDGE_CURVE('',#4037,#4045,#2517,.T.);
#4891=EDGE_CURVE('',#4046,#4045,#2518,.T.);
#4892=EDGE_CURVE('',#4038,#4046,#2519,.T.);
#4893=EDGE_CURVE('',#4031,#4046,#2520,.T.);
#4894=EDGE_CURVE('',#4047,#4032,#2521,.T.);
#4895=EDGE_CURVE('',#4039,#4047,#2522,.T.);
#4896=EDGE_CURVE('',#4048,#4047,#2523,.T.);
#4897=EDGE_CURVE('',#4040,#4048,#2524,.T.);
#4898=EDGE_CURVE('',#4049,#4048,#2525,.T.);
#4899=EDGE_CURVE('',#4041,#4049,#2526,.T.);
#4900=EDGE_CURVE('',#4050,#4049,#2527,.T.);
#4901=EDGE_CURVE('',#4042,#4050,#2528,.T.);
#4902=EDGE_CURVE('',#4029,#4050,#2529,.T.);
#4903=EDGE_CURVE('',#4051,#4052,#2530,.T.);
#4904=EDGE_CURVE('',#4052,#4053,#2531,.T.);
#4905=EDGE_CURVE('',#4054,#4053,#2532,.T.);
#4906=EDGE_CURVE('',#4051,#4054,#2533,.T.);
#4907=EDGE_CURVE('',#4055,#4051,#2534,.T.);
#4908=EDGE_CURVE('',#4056,#4054,#2535,.T.);
#4909=EDGE_CURVE('',#4055,#4056,#2536,.T.);
#4910=EDGE_CURVE('',#4057,#4055,#2537,.T.);
#4911=EDGE_CURVE('',#4058,#4056,#2538,.T.);
#4912=EDGE_CURVE('',#4057,#4058,#2539,.T.);
#4913=EDGE_CURVE('',#4059,#4057,#2540,.T.);
#4914=EDGE_CURVE('',#4060,#4058,#2541,.T.);
#4915=EDGE_CURVE('',#4059,#4060,#2542,.T.);
#4916=EDGE_CURVE('',#4061,#4059,#2543,.T.);
#4917=EDGE_CURVE('',#4062,#4060,#2544,.T.);
#4918=EDGE_CURVE('',#4061,#4062,#2545,.T.);
#4919=EDGE_CURVE('',#4063,#4061,#2546,.T.);
#4920=EDGE_CURVE('',#4064,#4062,#2547,.T.);
#4921=EDGE_CURVE('',#4063,#4064,#2548,.T.);
#4922=EDGE_CURVE('',#4065,#4063,#2549,.T.);
#4923=EDGE_CURVE('',#4066,#4064,#2550,.T.);
#4924=EDGE_CURVE('',#4065,#4066,#2551,.T.);
#4925=EDGE_CURVE('',#4052,#4065,#2552,.T.);
#4926=EDGE_CURVE('',#4053,#4066,#2553,.T.);
#4927=EDGE_CURVE('',#4067,#4068,#2554,.T.);
#4928=EDGE_CURVE('',#4067,#4069,#2555,.T.);
#4929=EDGE_CURVE('',#4070,#4069,#2556,.T.);
#4930=EDGE_CURVE('',#4068,#4070,#2557,.T.);
#4931=EDGE_CURVE('',#4068,#4071,#2558,.T.);
#4932=EDGE_CURVE('',#4072,#4070,#2559,.T.);
#4933=EDGE_CURVE('',#4071,#4072,#2560,.T.);
#4934=EDGE_CURVE('',#4071,#4073,#2561,.T.);
#4935=EDGE_CURVE('',#4074,#4072,#2562,.T.);
#4936=EDGE_CURVE('',#4073,#4074,#2563,.T.);
#4937=EDGE_CURVE('',#4073,#4075,#2564,.T.);
#4938=EDGE_CURVE('',#4076,#4074,#2565,.T.);
#4939=EDGE_CURVE('',#4075,#4076,#2566,.T.);
#4940=EDGE_CURVE('',#4075,#4077,#2567,.T.);
#4941=EDGE_CURVE('',#4078,#4076,#2568,.T.);
#4942=EDGE_CURVE('',#4077,#4078,#2569,.T.);
#4943=EDGE_CURVE('',#4077,#4079,#2570,.T.);
#4944=EDGE_CURVE('',#4080,#4078,#2571,.T.);
#4945=EDGE_CURVE('',#4079,#4080,#2572,.T.);
#4946=EDGE_CURVE('',#4079,#4081,#2573,.T.);
#4947=EDGE_CURVE('',#4082,#4080,#2574,.T.);
#4948=EDGE_CURVE('',#4081,#4082,#2575,.T.);
#4949=EDGE_CURVE('',#4081,#4067,#2576,.T.);
#4950=EDGE_CURVE('',#4069,#4082,#2577,.T.);
#4951=EDGE_CURVE('',#4083,#4083,#3529,.T.);
#4952=EDGE_CURVE('',#4083,#4084,#2578,.T.);
#4953=EDGE_CURVE('',#4084,#4084,#3530,.T.);
#4954=EDGE_CURVE('',#4084,#4085,#2579,.T.);
#4955=EDGE_CURVE('',#4085,#4085,#3531,.T.);
#4956=EDGE_CURVE('',#4086,#4086,#3532,.T.);
#4957=EDGE_CURVE('',#4086,#4087,#2580,.T.);
#4958=EDGE_CURVE('',#4087,#4087,#3533,.T.);
#4959=EDGE_CURVE('',#4088,#4088,#3534,.T.);
#4960=EDGE_CURVE('',#4089,#4089,#3535,.T.);
#4961=EDGE_CURVE('',#4089,#4088,#2581,.T.);
#4962=EDGE_CURVE('',#4090,#4090,#3536,.T.);
#4963=EDGE_CURVE('',#4090,#4089,#2582,.T.);
#4964=EDGE_CURVE('',#4091,#4091,#3537,.T.);
#4965=EDGE_CURVE('',#4091,#4090,#2583,.T.);
#4966=EDGE_CURVE('',#4092,#4092,#3538,.T.);
#4967=EDGE_CURVE('',#4093,#4093,#3539,.F.);
#4968=EDGE_CURVE('',#4093,#4092,#2584,.T.);
#4969=EDGE_CURVE('',#4094,#4094,#3540,.F.);
#4970=EDGE_CURVE('',#4094,#4093,#2585,.T.);
#4971=EDGE_CURVE('',#4095,#4095,#3541,.T.);
#4972=EDGE_CURVE('',#4095,#4094,#2586,.T.);
#4973=EDGE_CURVE('',#4096,#4097,#2587,.T.);
#4974=EDGE_CURVE('',#4097,#4098,#2588,.T.);
#4975=EDGE_CURVE('',#4098,#4099,#2589,.T.);
#4976=EDGE_CURVE('',#4096,#4099,#2590,.T.);
#4977=EDGE_CURVE('',#4097,#4100,#2591,.T.);
#4978=EDGE_CURVE('',#4100,#4101,#2592,.T.);
#4979=EDGE_CURVE('',#4101,#4098,#2593,.T.);
#4980=EDGE_CURVE('',#4100,#4102,#2594,.T.);
#4981=EDGE_CURVE('',#4102,#4103,#2595,.T.);
#4982=EDGE_CURVE('',#4103,#4101,#2596,.T.);
#4983=EDGE_CURVE('',#4102,#4104,#2597,.T.);
#4984=EDGE_CURVE('',#4104,#4105,#2598,.T.);
#4985=EDGE_CURVE('',#4105,#4103,#2599,.T.);
#4986=EDGE_CURVE('',#4104,#4106,#2600,.T.);
#4987=EDGE_CURVE('',#4106,#4107,#2601,.T.);
#4988=EDGE_CURVE('',#4107,#4105,#2602,.T.);
#4989=EDGE_CURVE('',#4106,#4096,#2603,.T.);
#4990=EDGE_CURVE('',#4099,#4107,#2604,.T.);
#4991=EDGE_CURVE('',#4108,#4108,#3542,.T.);
#4992=EDGE_CURVE('',#4108,#4109,#2605,.T.);
#4993=EDGE_CURVE('',#4109,#4109,#3543,.T.);
#4994=EDGE_CURVE('',#4110,#4110,#3544,.T.);
#4995=EDGE_CURVE('',#4110,#4111,#2606,.T.);
#4996=EDGE_CURVE('',#4111,#4111,#3545,.T.);
#4997=EDGE_CURVE('',#4112,#4112,#3546,.T.);
#4998=EDGE_CURVE('',#4113,#4113,#3547,.T.);
#4999=EDGE_CURVE('',#4113,#4112,#2607,.T.);
#5000=EDGE_CURVE('',#4114,#4114,#3548,.T.);
#5001=EDGE_CURVE('',#4114,#4113,#2608,.T.);
#5002=EDGE_CURVE('',#4115,#4115,#3549,.T.);
#5003=EDGE_CURVE('',#4115,#4114,#2609,.T.);
#5004=EDGE_CURVE('',#4116,#4116,#3550,.T.);
#5005=EDGE_CURVE('',#4117,#4117,#3551,.F.);
#5006=EDGE_CURVE('',#4117,#4116,#2610,.T.);
#5007=EDGE_CURVE('',#4118,#4118,#3552,.F.);
#5008=EDGE_CURVE('',#4118,#4117,#2611,.T.);
#5009=EDGE_CURVE('',#4119,#4119,#3553,.T.);
#5010=EDGE_CURVE('',#4119,#4118,#2612,.T.);
#5011=EDGE_CURVE('',#4120,#4121,#2613,.T.);
#5012=EDGE_CURVE('',#4121,#4122,#2614,.T.);
#5013=EDGE_CURVE('',#4122,#4123,#2615,.T.);
#5014=EDGE_CURVE('',#4120,#4123,#2616,.T.);
#5015=EDGE_CURVE('',#4121,#4124,#2617,.T.);
#5016=EDGE_CURVE('',#4124,#4125,#2618,.T.);
#5017=EDGE_CURVE('',#4125,#4122,#2619,.T.);
#5018=EDGE_CURVE('',#4124,#4126,#2620,.T.);
#5019=EDGE_CURVE('',#4126,#4127,#2621,.T.);
#5020=EDGE_CURVE('',#4127,#4125,#2622,.T.);
#5021=EDGE_CURVE('',#4126,#4128,#2623,.T.);
#5022=EDGE_CURVE('',#4128,#4129,#2624,.T.);
#5023=EDGE_CURVE('',#4129,#4127,#2625,.T.);
#5024=EDGE_CURVE('',#4128,#4130,#2626,.T.);
#5025=EDGE_CURVE('',#4130,#4131,#2627,.T.);
#5026=EDGE_CURVE('',#4131,#4129,#2628,.T.);
#5027=EDGE_CURVE('',#4130,#4120,#2629,.T.);
#5028=EDGE_CURVE('',#4123,#4131,#2630,.T.);
#5029=EDGE_CURVE('',#4132,#4132,#3554,.T.);
#5030=EDGE_CURVE('',#4132,#4133,#2631,.T.);
#5031=EDGE_CURVE('',#4133,#4133,#3555,.T.);
#5032=EDGE_CURVE('',#4133,#4134,#2632,.T.);
#5033=EDGE_CURVE('',#4134,#4134,#3556,.T.);
#5034=EDGE_CURVE('',#4135,#4135,#3557,.T.);
#5035=EDGE_CURVE('',#4135,#4136,#2633,.T.);
#5036=EDGE_CURVE('',#4136,#4136,#3558,.T.);
#5037=EDGE_CURVE('',#4137,#4138,#2634,.T.);
#5038=EDGE_CURVE('',#4138,#4139,#2635,.T.);
#5039=EDGE_CURVE('',#4139,#4140,#2636,.T.);
#5040=EDGE_CURVE('',#4137,#4140,#2637,.T.);
#5041=EDGE_CURVE('',#4138,#4141,#2638,.T.);
#5042=EDGE_CURVE('',#4141,#4142,#2639,.T.);
#5043=EDGE_CURVE('',#4142,#4139,#2640,.T.);
#5044=EDGE_CURVE('',#4141,#4143,#2641,.T.);
#5045=EDGE_CURVE('',#4143,#4144,#2642,.T.);
#5046=EDGE_CURVE('',#4144,#4142,#2643,.T.);
#5047=EDGE_CURVE('',#4143,#4145,#2644,.T.);
#5048=EDGE_CURVE('',#4145,#4146,#2645,.T.);
#5049=EDGE_CURVE('',#4146,#4144,#2646,.T.);
#5050=EDGE_CURVE('',#4145,#4147,#2647,.T.);
#5051=EDGE_CURVE('',#4147,#4148,#2648,.T.);
#5052=EDGE_CURVE('',#4148,#4146,#2649,.T.);
#5053=EDGE_CURVE('',#4147,#4137,#2650,.T.);
#5054=EDGE_CURVE('',#4140,#4148,#2651,.T.);
#5055=EDGE_CURVE('',#4149,#4149,#3559,.T.);
#5056=EDGE_CURVE('',#4150,#4150,#3560,.T.);
#5057=EDGE_CURVE('',#4151,#4151,#3561,.T.);
#5058=EDGE_CURVE('',#4151,#4150,#2652,.T.);
#5059=EDGE_CURVE('',#4152,#4152,#3562,.T.);
#5060=EDGE_CURVE('',#4152,#4151,#2653,.T.);
#5061=EDGE_CURVE('',#4153,#4153,#3563,.T.);
#5062=EDGE_CURVE('',#4153,#4152,#2654,.T.);
#5063=EDGE_CURVE('',#4154,#4154,#3564,.T.);
#5064=EDGE_CURVE('',#4155,#4155,#3565,.F.);
#5065=EDGE_CURVE('',#4155,#4154,#2655,.T.);
#5066=EDGE_CURVE('',#4149,#4155,#2656,.T.);
#5067=ORIENTED_EDGE('',*,*,#4156,.F.);
#5068=ORIENTED_EDGE('',*,*,#4157,.T.);
#5069=ORIENTED_EDGE('',*,*,#4158,.F.);
#5070=ORIENTED_EDGE('',*,*,#4157,.F.);
#5071=ORIENTED_EDGE('',*,*,#4159,.F.);
#5072=ORIENTED_EDGE('',*,*,#4160,.T.);
#5073=ORIENTED_EDGE('',*,*,#4161,.F.);
#5074=ORIENTED_EDGE('',*,*,#4160,.F.);
#5075=ORIENTED_EDGE('',*,*,#4162,.F.);
#5076=ORIENTED_EDGE('',*,*,#4163,.T.);
#5077=ORIENTED_EDGE('',*,*,#4164,.F.);
#5078=ORIENTED_EDGE('',*,*,#4163,.F.);
#5079=ORIENTED_EDGE('',*,*,#4165,.F.);
#5080=ORIENTED_EDGE('',*,*,#4166,.T.);
#5081=ORIENTED_EDGE('',*,*,#4167,.F.);
#5082=ORIENTED_EDGE('',*,*,#4166,.F.);
#5083=ORIENTED_EDGE('',*,*,#4168,.F.);
#5084=ORIENTED_EDGE('',*,*,#4169,.T.);
#5085=ORIENTED_EDGE('',*,*,#4170,.F.);
#5086=ORIENTED_EDGE('',*,*,#4169,.F.);
#5087=ORIENTED_EDGE('',*,*,#4171,.F.);
#5088=ORIENTED_EDGE('',*,*,#4172,.T.);
#5089=ORIENTED_EDGE('',*,*,#4173,.F.);
#5090=ORIENTED_EDGE('',*,*,#4172,.F.);
#5091=ORIENTED_EDGE('',*,*,#4174,.T.);
#5092=ORIENTED_EDGE('',*,*,#4175,.T.);
#5093=ORIENTED_EDGE('',*,*,#4176,.F.);
#5094=ORIENTED_EDGE('',*,*,#4177,.F.);
#5095=ORIENTED_EDGE('',*,*,#4178,.T.);
#5096=ORIENTED_EDGE('',*,*,#4177,.T.);
#5097=ORIENTED_EDGE('',*,*,#4179,.F.);
#5098=ORIENTED_EDGE('',*,*,#4180,.F.);
#5099=ORIENTED_EDGE('',*,*,#4181,.T.);
#5100=ORIENTED_EDGE('',*,*,#4180,.T.);
#5101=ORIENTED_EDGE('',*,*,#4182,.F.);
#5102=ORIENTED_EDGE('',*,*,#4183,.F.);
#5103=ORIENTED_EDGE('',*,*,#4184,.T.);
#5104=ORIENTED_EDGE('',*,*,#4183,.T.);
#5105=ORIENTED_EDGE('',*,*,#4185,.F.);
#5106=ORIENTED_EDGE('',*,*,#4175,.F.);
#5107=ORIENTED_EDGE('',*,*,#4185,.T.);
#5108=ORIENTED_EDGE('',*,*,#4182,.T.);
#5109=ORIENTED_EDGE('',*,*,#4179,.T.);
#5110=ORIENTED_EDGE('',*,*,#4176,.T.);
#5111=ORIENTED_EDGE('',*,*,#4173,.T.);
#5112=ORIENTED_EDGE('',*,*,#4170,.T.);
#5113=ORIENTED_EDGE('',*,*,#4167,.T.);
#5114=ORIENTED_EDGE('',*,*,#4164,.T.);
#5115=ORIENTED_EDGE('',*,*,#4161,.T.);
#5116=ORIENTED_EDGE('',*,*,#4158,.T.);
#5117=ORIENTED_EDGE('',*,*,#4184,.F.);
#5118=ORIENTED_EDGE('',*,*,#4174,.F.);
#5119=ORIENTED_EDGE('',*,*,#4178,.F.);
#5120=ORIENTED_EDGE('',*,*,#4181,.F.);
#5121=ORIENTED_EDGE('',*,*,#4171,.T.);
#5122=ORIENTED_EDGE('',*,*,#4168,.T.);
#5123=ORIENTED_EDGE('',*,*,#4165,.T.);
#5124=ORIENTED_EDGE('',*,*,#4162,.T.);
#5125=ORIENTED_EDGE('',*,*,#4159,.T.);
#5126=ORIENTED_EDGE('',*,*,#4156,.T.);
#5127=ORIENTED_EDGE('',*,*,#4186,.F.);
#5128=ORIENTED_EDGE('',*,*,#4187,.T.);
#5129=ORIENTED_EDGE('',*,*,#4188,.F.);
#5130=ORIENTED_EDGE('',*,*,#4187,.F.);
#5131=ORIENTED_EDGE('',*,*,#4189,.F.);
#5132=ORIENTED_EDGE('',*,*,#4190,.T.);
#5133=ORIENTED_EDGE('',*,*,#4191,.F.);
#5134=ORIENTED_EDGE('',*,*,#4190,.F.);
#5135=ORIENTED_EDGE('',*,*,#4192,.F.);
#5136=ORIENTED_EDGE('',*,*,#4193,.T.);
#5137=ORIENTED_EDGE('',*,*,#4194,.F.);
#5138=ORIENTED_EDGE('',*,*,#4193,.F.);
#5139=ORIENTED_EDGE('',*,*,#4195,.F.);
#5140=ORIENTED_EDGE('',*,*,#4196,.T.);
#5141=ORIENTED_EDGE('',*,*,#4197,.F.);
#5142=ORIENTED_EDGE('',*,*,#4196,.F.);
#5143=ORIENTED_EDGE('',*,*,#4198,.F.);
#5144=ORIENTED_EDGE('',*,*,#4199,.T.);
#5145=ORIENTED_EDGE('',*,*,#4200,.F.);
#5146=ORIENTED_EDGE('',*,*,#4199,.F.);
#5147=ORIENTED_EDGE('',*,*,#4201,.F.);
#5148=ORIENTED_EDGE('',*,*,#4202,.T.);
#5149=ORIENTED_EDGE('',*,*,#4203,.F.);
#5150=ORIENTED_EDGE('',*,*,#4202,.F.);
#5151=ORIENTED_EDGE('',*,*,#4204,.T.);
#5152=ORIENTED_EDGE('',*,*,#4205,.T.);
#5153=ORIENTED_EDGE('',*,*,#4206,.F.);
#5154=ORIENTED_EDGE('',*,*,#4207,.F.);
#5155=ORIENTED_EDGE('',*,*,#4208,.T.);
#5156=ORIENTED_EDGE('',*,*,#4207,.T.);
#5157=ORIENTED_EDGE('',*,*,#4209,.F.);
#5158=ORIENTED_EDGE('',*,*,#4210,.F.);
#5159=ORIENTED_EDGE('',*,*,#4211,.T.);
#5160=ORIENTED_EDGE('',*,*,#4210,.T.);
#5161=ORIENTED_EDGE('',*,*,#4212,.F.);
#5162=ORIENTED_EDGE('',*,*,#4213,.F.);
#5163=ORIENTED_EDGE('',*,*,#4214,.T.);
#5164=ORIENTED_EDGE('',*,*,#4213,.T.);
#5165=ORIENTED_EDGE('',*,*,#4215,.F.);
#5166=ORIENTED_EDGE('',*,*,#4205,.F.);
#5167=ORIENTED_EDGE('',*,*,#4215,.T.);
#5168=ORIENTED_EDGE('',*,*,#4212,.T.);
#5169=ORIENTED_EDGE('',*,*,#4209,.T.);
#5170=ORIENTED_EDGE('',*,*,#4206,.T.);
#5171=ORIENTED_EDGE('',*,*,#4203,.T.);
#5172=ORIENTED_EDGE('',*,*,#4200,.T.);
#5173=ORIENTED_EDGE('',*,*,#4197,.T.);
#5174=ORIENTED_EDGE('',*,*,#4194,.T.);
#5175=ORIENTED_EDGE('',*,*,#4191,.T.);
#5176=ORIENTED_EDGE('',*,*,#4188,.T.);
#5177=ORIENTED_EDGE('',*,*,#4214,.F.);
#5178=ORIENTED_EDGE('',*,*,#4204,.F.);
#5179=ORIENTED_EDGE('',*,*,#4208,.F.);
#5180=ORIENTED_EDGE('',*,*,#4211,.F.);
#5181=ORIENTED_EDGE('',*,*,#4201,.T.);
#5182=ORIENTED_EDGE('',*,*,#4198,.T.);
#5183=ORIENTED_EDGE('',*,*,#4195,.T.);
#5184=ORIENTED_EDGE('',*,*,#4192,.T.);
#5185=ORIENTED_EDGE('',*,*,#4189,.T.);
#5186=ORIENTED_EDGE('',*,*,#4186,.T.);
#5187=ORIENTED_EDGE('',*,*,#4216,.F.);
#5188=ORIENTED_EDGE('',*,*,#4217,.T.);
#5189=ORIENTED_EDGE('',*,*,#4218,.F.);
#5190=ORIENTED_EDGE('',*,*,#4217,.F.);
#5191=ORIENTED_EDGE('',*,*,#4219,.F.);
#5192=ORIENTED_EDGE('',*,*,#4220,.T.);
#5193=ORIENTED_EDGE('',*,*,#4221,.F.);
#5194=ORIENTED_EDGE('',*,*,#4220,.F.);
#5195=ORIENTED_EDGE('',*,*,#4222,.T.);
#5196=ORIENTED_EDGE('',*,*,#4223,.T.);
#5197=ORIENTED_EDGE('',*,*,#4224,.F.);
#5198=ORIENTED_EDGE('',*,*,#4225,.F.);
#5199=ORIENTED_EDGE('',*,*,#4226,.T.);
#5200=ORIENTED_EDGE('',*,*,#4225,.T.);
#5201=ORIENTED_EDGE('',*,*,#4227,.F.);
#5202=ORIENTED_EDGE('',*,*,#4228,.F.);
#5203=ORIENTED_EDGE('',*,*,#4229,.T.);
#5204=ORIENTED_EDGE('',*,*,#4228,.T.);
#5205=ORIENTED_EDGE('',*,*,#4230,.F.);
#5206=ORIENTED_EDGE('',*,*,#4231,.F.);
#5207=ORIENTED_EDGE('',*,*,#4232,.T.);
#5208=ORIENTED_EDGE('',*,*,#4231,.T.);
#5209=ORIENTED_EDGE('',*,*,#4233,.F.);
#5210=ORIENTED_EDGE('',*,*,#4223,.F.);
#5211=ORIENTED_EDGE('',*,*,#4233,.T.);
#5212=ORIENTED_EDGE('',*,*,#4230,.T.);
#5213=ORIENTED_EDGE('',*,*,#4227,.T.);
#5214=ORIENTED_EDGE('',*,*,#4224,.T.);
#5215=ORIENTED_EDGE('',*,*,#4218,.T.);
#5216=ORIENTED_EDGE('',*,*,#4221,.T.);
#5217=ORIENTED_EDGE('',*,*,#4232,.F.);
#5218=ORIENTED_EDGE('',*,*,#4222,.F.);
#5219=ORIENTED_EDGE('',*,*,#4226,.F.);
#5220=ORIENTED_EDGE('',*,*,#4229,.F.);
#5221=ORIENTED_EDGE('',*,*,#4216,.T.);
#5222=ORIENTED_EDGE('',*,*,#4219,.T.);
#5223=ORIENTED_EDGE('',*,*,#4234,.F.);
#5224=ORIENTED_EDGE('',*,*,#4235,.T.);
#5225=ORIENTED_EDGE('',*,*,#4236,.F.);
#5226=ORIENTED_EDGE('',*,*,#4235,.F.);
#5227=ORIENTED_EDGE('',*,*,#4237,.F.);
#5228=ORIENTED_EDGE('',*,*,#4238,.T.);
#5229=ORIENTED_EDGE('',*,*,#4239,.F.);
#5230=ORIENTED_EDGE('',*,*,#4238,.F.);
#5231=ORIENTED_EDGE('',*,*,#4240,.T.);
#5232=ORIENTED_EDGE('',*,*,#4241,.T.);
#5233=ORIENTED_EDGE('',*,*,#4242,.F.);
#5234=ORIENTED_EDGE('',*,*,#4243,.F.);
#5235=ORIENTED_EDGE('',*,*,#4244,.T.);
#5236=ORIENTED_EDGE('',*,*,#4243,.T.);
#5237=ORIENTED_EDGE('',*,*,#4245,.F.);
#5238=ORIENTED_EDGE('',*,*,#4246,.F.);
#5239=ORIENTED_EDGE('',*,*,#4247,.T.);
#5240=ORIENTED_EDGE('',*,*,#4246,.T.);
#5241=ORIENTED_EDGE('',*,*,#4248,.F.);
#5242=ORIENTED_EDGE('',*,*,#4249,.F.);
#5243=ORIENTED_EDGE('',*,*,#4250,.T.);
#5244=ORIENTED_EDGE('',*,*,#4249,.T.);
#5245=ORIENTED_EDGE('',*,*,#4251,.F.);
#5246=ORIENTED_EDGE('',*,*,#4241,.F.);
#5247=ORIENTED_EDGE('',*,*,#4251,.T.);
#5248=ORIENTED_EDGE('',*,*,#4248,.T.);
#5249=ORIENTED_EDGE('',*,*,#4245,.T.);
#5250=ORIENTED_EDGE('',*,*,#4242,.T.);
#5251=ORIENTED_EDGE('',*,*,#4236,.T.);
#5252=ORIENTED_EDGE('',*,*,#4239,.T.);
#5253=ORIENTED_EDGE('',*,*,#4250,.F.);
#5254=ORIENTED_EDGE('',*,*,#4240,.F.);
#5255=ORIENTED_EDGE('',*,*,#4244,.F.);
#5256=ORIENTED_EDGE('',*,*,#4247,.F.);
#5257=ORIENTED_EDGE('',*,*,#4234,.T.);
#5258=ORIENTED_EDGE('',*,*,#4237,.T.);
#5259=ORIENTED_EDGE('',*,*,#4252,.T.);
#5260=ORIENTED_EDGE('',*,*,#4253,.T.);
#5261=ORIENTED_EDGE('',*,*,#4254,.F.);
#5262=ORIENTED_EDGE('',*,*,#4255,.F.);
#5263=ORIENTED_EDGE('',*,*,#4256,.T.);
#5264=ORIENTED_EDGE('',*,*,#4255,.T.);
#5265=ORIENTED_EDGE('',*,*,#4257,.F.);
#5266=ORIENTED_EDGE('',*,*,#4258,.F.);
#5267=ORIENTED_EDGE('',*,*,#4259,.T.);
#5268=ORIENTED_EDGE('',*,*,#4258,.T.);
#5269=ORIENTED_EDGE('',*,*,#4260,.F.);
#5270=ORIENTED_EDGE('',*,*,#4261,.F.);
#5271=ORIENTED_EDGE('',*,*,#4262,.T.);
#5272=ORIENTED_EDGE('',*,*,#4261,.T.);
#5273=ORIENTED_EDGE('',*,*,#4263,.F.);
#5274=ORIENTED_EDGE('',*,*,#4253,.F.);
#5275=ORIENTED_EDGE('',*,*,#4263,.T.);
#5276=ORIENTED_EDGE('',*,*,#4260,.T.);
#5277=ORIENTED_EDGE('',*,*,#4257,.T.);
#5278=ORIENTED_EDGE('',*,*,#4254,.T.);
#5279=ORIENTED_EDGE('',*,*,#4262,.F.);
#5280=ORIENTED_EDGE('',*,*,#4252,.F.);
#5281=ORIENTED_EDGE('',*,*,#4256,.F.);
#5282=ORIENTED_EDGE('',*,*,#4259,.F.);
#5283=ORIENTED_EDGE('',*,*,#4264,.T.);
#5284=ORIENTED_EDGE('',*,*,#4265,.T.);
#5285=ORIENTED_EDGE('',*,*,#4266,.F.);
#5286=ORIENTED_EDGE('',*,*,#4267,.F.);
#5287=ORIENTED_EDGE('',*,*,#4268,.T.);
#5288=ORIENTED_EDGE('',*,*,#4267,.T.);
#5289=ORIENTED_EDGE('',*,*,#4269,.F.);
#5290=ORIENTED_EDGE('',*,*,#4270,.F.);
#5291=ORIENTED_EDGE('',*,*,#4271,.T.);
#5292=ORIENTED_EDGE('',*,*,#4270,.T.);
#5293=ORIENTED_EDGE('',*,*,#4272,.F.);
#5294=ORIENTED_EDGE('',*,*,#4273,.F.);
#5295=ORIENTED_EDGE('',*,*,#4274,.T.);
#5296=ORIENTED_EDGE('',*,*,#4273,.T.);
#5297=ORIENTED_EDGE('',*,*,#4275,.F.);
#5298=ORIENTED_EDGE('',*,*,#4265,.F.);
#5299=ORIENTED_EDGE('',*,*,#4275,.T.);
#5300=ORIENTED_EDGE('',*,*,#4272,.T.);
#5301=ORIENTED_EDGE('',*,*,#4269,.T.);
#5302=ORIENTED_EDGE('',*,*,#4266,.T.);
#5303=ORIENTED_EDGE('',*,*,#4274,.F.);
#5304=ORIENTED_EDGE('',*,*,#4264,.F.);
#5305=ORIENTED_EDGE('',*,*,#4268,.F.);
#5306=ORIENTED_EDGE('',*,*,#4271,.F.);
#5307=ORIENTED_EDGE('',*,*,#4276,.F.);
#5308=ORIENTED_EDGE('',*,*,#4277,.T.);
#5309=ORIENTED_EDGE('',*,*,#4278,.F.);
#5310=ORIENTED_EDGE('',*,*,#4277,.F.);
#5311=ORIENTED_EDGE('',*,*,#4279,.F.);
#5312=ORIENTED_EDGE('',*,*,#4280,.T.);
#5313=ORIENTED_EDGE('',*,*,#4281,.F.);
#5314=ORIENTED_EDGE('',*,*,#4280,.F.);
#5315=ORIENTED_EDGE('',*,*,#4282,.T.);
#5316=ORIENTED_EDGE('',*,*,#4283,.T.);
#5317=ORIENTED_EDGE('',*,*,#4284,.F.);
#5318=ORIENTED_EDGE('',*,*,#4285,.F.);
#5319=ORIENTED_EDGE('',*,*,#4286,.T.);
#5320=ORIENTED_EDGE('',*,*,#4285,.T.);
#5321=ORIENTED_EDGE('',*,*,#4287,.F.);
#5322=ORIENTED_EDGE('',*,*,#4288,.F.);
#5323=ORIENTED_EDGE('',*,*,#4289,.T.);
#5324=ORIENTED_EDGE('',*,*,#4288,.T.);
#5325=ORIENTED_EDGE('',*,*,#4290,.F.);
#5326=ORIENTED_EDGE('',*,*,#4291,.F.);
#5327=ORIENTED_EDGE('',*,*,#4292,.T.);
#5328=ORIENTED_EDGE('',*,*,#4291,.T.);
#5329=ORIENTED_EDGE('',*,*,#4293,.F.);
#5330=ORIENTED_EDGE('',*,*,#4283,.F.);
#5331=ORIENTED_EDGE('',*,*,#4293,.T.);
#5332=ORIENTED_EDGE('',*,*,#4290,.T.);
#5333=ORIENTED_EDGE('',*,*,#4287,.T.);
#5334=ORIENTED_EDGE('',*,*,#4284,.T.);
#5335=ORIENTED_EDGE('',*,*,#4278,.T.);
#5336=ORIENTED_EDGE('',*,*,#4281,.T.);
#5337=ORIENTED_EDGE('',*,*,#4292,.F.);
#5338=ORIENTED_EDGE('',*,*,#4282,.F.);
#5339=ORIENTED_EDGE('',*,*,#4286,.F.);
#5340=ORIENTED_EDGE('',*,*,#4289,.F.);
#5341=ORIENTED_EDGE('',*,*,#4276,.T.);
#5342=ORIENTED_EDGE('',*,*,#4279,.T.);
#5343=ORIENTED_EDGE('',*,*,#4294,.F.);
#5344=ORIENTED_EDGE('',*,*,#4295,.T.);
#5345=ORIENTED_EDGE('',*,*,#4296,.F.);
#5346=ORIENTED_EDGE('',*,*,#4295,.F.);
#5347=ORIENTED_EDGE('',*,*,#4297,.F.);
#5348=ORIENTED_EDGE('',*,*,#4298,.T.);
#5349=ORIENTED_EDGE('',*,*,#4299,.F.);
#5350=ORIENTED_EDGE('',*,*,#4298,.F.);
#5351=ORIENTED_EDGE('',*,*,#4300,.T.);
#5352=ORIENTED_EDGE('',*,*,#4301,.T.);
#5353=ORIENTED_EDGE('',*,*,#4302,.F.);
#5354=ORIENTED_EDGE('',*,*,#4303,.F.);
#5355=ORIENTED_EDGE('',*,*,#4304,.T.);
#5356=ORIENTED_EDGE('',*,*,#4303,.T.);
#5357=ORIENTED_EDGE('',*,*,#4305,.F.);
#5358=ORIENTED_EDGE('',*,*,#4306,.F.);
#5359=ORIENTED_EDGE('',*,*,#4307,.T.);
#5360=ORIENTED_EDGE('',*,*,#4306,.T.);
#5361=ORIENTED_EDGE('',*,*,#4308,.F.);
#5362=ORIENTED_EDGE('',*,*,#4309,.F.);
#5363=ORIENTED_EDGE('',*,*,#4310,.T.);
#5364=ORIENTED_EDGE('',*,*,#4309,.T.);
#5365=ORIENTED_EDGE('',*,*,#4311,.F.);
#5366=ORIENTED_EDGE('',*,*,#4301,.F.);
#5367=ORIENTED_EDGE('',*,*,#4311,.T.);
#5368=ORIENTED_EDGE('',*,*,#4308,.T.);
#5369=ORIENTED_EDGE('',*,*,#4305,.T.);
#5370=ORIENTED_EDGE('',*,*,#4302,.T.);
#5371=ORIENTED_EDGE('',*,*,#4296,.T.);
#5372=ORIENTED_EDGE('',*,*,#4299,.T.);
#5373=ORIENTED_EDGE('',*,*,#4310,.F.);
#5374=ORIENTED_EDGE('',*,*,#4300,.F.);
#5375=ORIENTED_EDGE('',*,*,#4304,.F.);
#5376=ORIENTED_EDGE('',*,*,#4307,.F.);
#5377=ORIENTED_EDGE('',*,*,#4294,.T.);
#5378=ORIENTED_EDGE('',*,*,#4297,.T.);
#5379=ORIENTED_EDGE('',*,*,#4312,.T.);
#5380=ORIENTED_EDGE('',*,*,#4313,.T.);
#5381=ORIENTED_EDGE('',*,*,#4314,.F.);
#5382=ORIENTED_EDGE('',*,*,#4315,.F.);
#5383=ORIENTED_EDGE('',*,*,#4316,.T.);
#5384=ORIENTED_EDGE('',*,*,#4315,.T.);
#5385=ORIENTED_EDGE('',*,*,#4317,.F.);
#5386=ORIENTED_EDGE('',*,*,#4318,.F.);
#5387=ORIENTED_EDGE('',*,*,#4319,.T.);
#5388=ORIENTED_EDGE('',*,*,#4318,.T.);
#5389=ORIENTED_EDGE('',*,*,#4320,.F.);
#5390=ORIENTED_EDGE('',*,*,#4321,.F.);
#5391=ORIENTED_EDGE('',*,*,#4322,.T.);
#5392=ORIENTED_EDGE('',*,*,#4321,.T.);
#5393=ORIENTED_EDGE('',*,*,#4323,.F.);
#5394=ORIENTED_EDGE('',*,*,#4313,.F.);
#5395=ORIENTED_EDGE('',*,*,#4323,.T.);
#5396=ORIENTED_EDGE('',*,*,#4320,.T.);
#5397=ORIENTED_EDGE('',*,*,#4317,.T.);
#5398=ORIENTED_EDGE('',*,*,#4314,.T.);
#5399=ORIENTED_EDGE('',*,*,#4322,.F.);
#5400=ORIENTED_EDGE('',*,*,#4312,.F.);
#5401=ORIENTED_EDGE('',*,*,#4316,.F.);
#5402=ORIENTED_EDGE('',*,*,#4319,.F.);
#5403=ORIENTED_EDGE('',*,*,#4324,.T.);
#5404=ORIENTED_EDGE('',*,*,#4325,.T.);
#5405=ORIENTED_EDGE('',*,*,#4326,.F.);
#5406=ORIENTED_EDGE('',*,*,#4327,.F.);
#5407=ORIENTED_EDGE('',*,*,#4328,.T.);
#5408=ORIENTED_EDGE('',*,*,#4327,.T.);
#5409=ORIENTED_EDGE('',*,*,#4329,.F.);
#5410=ORIENTED_EDGE('',*,*,#4330,.F.);
#5411=ORIENTED_EDGE('',*,*,#4331,.T.);
#5412=ORIENTED_EDGE('',*,*,#4330,.T.);
#5413=ORIENTED_EDGE('',*,*,#4332,.F.);
#5414=ORIENTED_EDGE('',*,*,#4333,.F.);
#5415=ORIENTED_EDGE('',*,*,#4334,.T.);
#5416=ORIENTED_EDGE('',*,*,#4333,.T.);
#5417=ORIENTED_EDGE('',*,*,#4335,.F.);
#5418=ORIENTED_EDGE('',*,*,#4325,.F.);
#5419=ORIENTED_EDGE('',*,*,#4335,.T.);
#5420=ORIENTED_EDGE('',*,*,#4332,.T.);
#5421=ORIENTED_EDGE('',*,*,#4329,.T.);
#5422=ORIENTED_EDGE('',*,*,#4326,.T.);
#5423=ORIENTED_EDGE('',*,*,#4334,.F.);
#5424=ORIENTED_EDGE('',*,*,#4324,.F.);
#5425=ORIENTED_EDGE('',*,*,#4328,.F.);
#5426=ORIENTED_EDGE('',*,*,#4331,.F.);
#5427=ORIENTED_EDGE('',*,*,#4336,.T.);
#5428=ORIENTED_EDGE('',*,*,#4337,.F.);
#5429=ORIENTED_EDGE('',*,*,#4338,.F.);
#5430=ORIENTED_EDGE('',*,*,#4339,.F.);
#5431=ORIENTED_EDGE('',*,*,#4340,.F.);
#5432=ORIENTED_EDGE('',*,*,#4341,.F.);
#5433=ORIENTED_EDGE('',*,*,#4342,.T.);
#5434=ORIENTED_EDGE('',*,*,#4343,.F.);
#5435=ORIENTED_EDGE('',*,*,#4341,.T.);
#5436=ORIENTED_EDGE('',*,*,#4339,.T.);
#5437=ORIENTED_EDGE('',*,*,#4344,.F.);
#5438=ORIENTED_EDGE('',*,*,#4345,.T.);
#5439=ORIENTED_EDGE('',*,*,#4346,.F.);
#5440=ORIENTED_EDGE('',*,*,#4347,.F.);
#5441=ORIENTED_EDGE('',*,*,#4348,.F.);
#5442=ORIENTED_EDGE('',*,*,#4349,.F.);
#5443=ORIENTED_EDGE('',*,*,#4350,.F.);
#5444=ORIENTED_EDGE('',*,*,#4351,.T.);
#5445=ORIENTED_EDGE('',*,*,#4352,.F.);
#5446=ORIENTED_EDGE('',*,*,#4350,.T.);
#5447=ORIENTED_EDGE('',*,*,#4348,.T.);
#5448=ORIENTED_EDGE('',*,*,#4353,.F.);
#5449=ORIENTED_EDGE('',*,*,#4346,.T.);
#5450=ORIENTED_EDGE('',*,*,#4354,.T.);
#5451=ORIENTED_EDGE('',*,*,#4355,.T.);
#5452=ORIENTED_EDGE('',*,*,#4356,.T.);
#5453=ORIENTED_EDGE('',*,*,#4337,.T.);
#5454=ORIENTED_EDGE('',*,*,#4357,.T.);
#5455=ORIENTED_EDGE('',*,*,#4352,.T.);
#5456=ORIENTED_EDGE('',*,*,#4358,.T.);
#5457=ORIENTED_EDGE('',*,*,#4343,.T.);
#5458=ORIENTED_EDGE('',*,*,#4359,.T.);
#5459=ORIENTED_EDGE('',*,*,#4360,.T.);
#5460=ORIENTED_EDGE('',*,*,#4361,.T.);
#5461=ORIENTED_EDGE('',*,*,#4362,.F.);
#5462=ORIENTED_EDGE('',*,*,#4363,.T.);
#5463=ORIENTED_EDGE('',*,*,#4344,.T.);
#5464=ORIENTED_EDGE('',*,*,#4363,.F.);
#5465=ORIENTED_EDGE('',*,*,#4364,.F.);
#5466=ORIENTED_EDGE('',*,*,#4365,.T.);
#5467=ORIENTED_EDGE('',*,*,#4353,.T.);
#5468=ORIENTED_EDGE('',*,*,#4365,.F.);
#5469=ORIENTED_EDGE('',*,*,#4366,.T.);
#5470=ORIENTED_EDGE('',*,*,#4367,.T.);
#5471=ORIENTED_EDGE('',*,*,#4355,.F.);
#5472=ORIENTED_EDGE('',*,*,#4368,.F.);
#5473=ORIENTED_EDGE('',*,*,#4369,.T.);
#5474=ORIENTED_EDGE('',*,*,#4368,.T.);
#5475=ORIENTED_EDGE('',*,*,#4354,.F.);
#5476=ORIENTED_EDGE('',*,*,#4345,.F.);
#5477=ORIENTED_EDGE('',*,*,#4349,.T.);
#5478=ORIENTED_EDGE('',*,*,#4357,.F.);
#5479=ORIENTED_EDGE('',*,*,#4336,.F.);
#5480=ORIENTED_EDGE('',*,*,#4340,.T.);
#5481=ORIENTED_EDGE('',*,*,#4361,.F.);
#5482=ORIENTED_EDGE('',*,*,#4370,.F.);
#5483=ORIENTED_EDGE('',*,*,#4371,.T.);
#5484=ORIENTED_EDGE('',*,*,#4370,.T.);
#5485=ORIENTED_EDGE('',*,*,#4360,.F.);
#5486=ORIENTED_EDGE('',*,*,#4372,.F.);
#5487=ORIENTED_EDGE('',*,*,#4373,.T.);
#5488=ORIENTED_EDGE('',*,*,#4372,.T.);
#5489=ORIENTED_EDGE('',*,*,#4359,.F.);
#5490=ORIENTED_EDGE('',*,*,#4342,.F.);
#5491=ORIENTED_EDGE('',*,*,#4338,.T.);
#5492=ORIENTED_EDGE('',*,*,#4358,.F.);
#5493=ORIENTED_EDGE('',*,*,#4351,.F.);
#5494=ORIENTED_EDGE('',*,*,#4347,.T.);
#5495=ORIENTED_EDGE('',*,*,#4356,.F.);
#5496=ORIENTED_EDGE('',*,*,#4367,.F.);
#5497=ORIENTED_EDGE('',*,*,#4373,.F.);
#5498=ORIENTED_EDGE('',*,*,#4366,.F.);
#5499=ORIENTED_EDGE('',*,*,#4369,.F.);
#5500=ORIENTED_EDGE('',*,*,#4371,.F.);
#5501=ORIENTED_EDGE('',*,*,#4362,.T.);
#5502=ORIENTED_EDGE('',*,*,#4364,.T.);
#5503=ORIENTED_EDGE('',*,*,#4374,.T.);
#5504=ORIENTED_EDGE('',*,*,#4375,.T.);
#5505=ORIENTED_EDGE('',*,*,#4376,.F.);
#5506=ORIENTED_EDGE('',*,*,#4377,.F.);
#5507=ORIENTED_EDGE('',*,*,#4378,.T.);
#5508=ORIENTED_EDGE('',*,*,#4377,.T.);
#5509=ORIENTED_EDGE('',*,*,#4379,.F.);
#5510=ORIENTED_EDGE('',*,*,#4380,.F.);
#5511=ORIENTED_EDGE('',*,*,#4381,.T.);
#5512=ORIENTED_EDGE('',*,*,#4380,.T.);
#5513=ORIENTED_EDGE('',*,*,#4382,.F.);
#5514=ORIENTED_EDGE('',*,*,#4383,.F.);
#5515=ORIENTED_EDGE('',*,*,#4384,.T.);
#5516=ORIENTED_EDGE('',*,*,#4383,.T.);
#5517=ORIENTED_EDGE('',*,*,#4385,.F.);
#5518=ORIENTED_EDGE('',*,*,#4375,.F.);
#5519=ORIENTED_EDGE('',*,*,#4385,.T.);
#5520=ORIENTED_EDGE('',*,*,#4382,.T.);
#5521=ORIENTED_EDGE('',*,*,#4379,.T.);
#5522=ORIENTED_EDGE('',*,*,#4376,.T.);
#5523=ORIENTED_EDGE('',*,*,#4384,.F.);
#5524=ORIENTED_EDGE('',*,*,#4374,.F.);
#5525=ORIENTED_EDGE('',*,*,#4378,.F.);
#5526=ORIENTED_EDGE('',*,*,#4381,.F.);
#5527=ORIENTED_EDGE('',*,*,#4386,.T.);
#5528=ORIENTED_EDGE('',*,*,#4387,.F.);
#5529=ORIENTED_EDGE('',*,*,#4388,.F.);
#5530=ORIENTED_EDGE('',*,*,#4389,.F.);
#5531=ORIENTED_EDGE('',*,*,#4390,.F.);
#5532=ORIENTED_EDGE('',*,*,#4391,.F.);
#5533=ORIENTED_EDGE('',*,*,#4392,.T.);
#5534=ORIENTED_EDGE('',*,*,#4393,.F.);
#5535=ORIENTED_EDGE('',*,*,#4391,.T.);
#5536=ORIENTED_EDGE('',*,*,#4389,.T.);
#5537=ORIENTED_EDGE('',*,*,#4394,.F.);
#5538=ORIENTED_EDGE('',*,*,#4395,.T.);
#5539=ORIENTED_EDGE('',*,*,#4396,.F.);
#5540=ORIENTED_EDGE('',*,*,#4397,.F.);
#5541=ORIENTED_EDGE('',*,*,#4398,.F.);
#5542=ORIENTED_EDGE('',*,*,#4399,.F.);
#5543=ORIENTED_EDGE('',*,*,#4400,.F.);
#5544=ORIENTED_EDGE('',*,*,#4401,.T.);
#5545=ORIENTED_EDGE('',*,*,#4402,.F.);
#5546=ORIENTED_EDGE('',*,*,#4400,.T.);
#5547=ORIENTED_EDGE('',*,*,#4398,.T.);
#5548=ORIENTED_EDGE('',*,*,#4403,.F.);
#5549=ORIENTED_EDGE('',*,*,#4396,.T.);
#5550=ORIENTED_EDGE('',*,*,#4404,.T.);
#5551=ORIENTED_EDGE('',*,*,#4405,.T.);
#5552=ORIENTED_EDGE('',*,*,#4406,.T.);
#5553=ORIENTED_EDGE('',*,*,#4387,.T.);
#5554=ORIENTED_EDGE('',*,*,#4407,.T.);
#5555=ORIENTED_EDGE('',*,*,#4402,.T.);
#5556=ORIENTED_EDGE('',*,*,#4408,.T.);
#5557=ORIENTED_EDGE('',*,*,#4393,.T.);
#5558=ORIENTED_EDGE('',*,*,#4409,.T.);
#5559=ORIENTED_EDGE('',*,*,#4410,.T.);
#5560=ORIENTED_EDGE('',*,*,#4411,.T.);
#5561=ORIENTED_EDGE('',*,*,#4412,.F.);
#5562=ORIENTED_EDGE('',*,*,#4413,.T.);
#5563=ORIENTED_EDGE('',*,*,#4394,.T.);
#5564=ORIENTED_EDGE('',*,*,#4413,.F.);
#5565=ORIENTED_EDGE('',*,*,#4414,.F.);
#5566=ORIENTED_EDGE('',*,*,#4415,.T.);
#5567=ORIENTED_EDGE('',*,*,#4403,.T.);
#5568=ORIENTED_EDGE('',*,*,#4415,.F.);
#5569=ORIENTED_EDGE('',*,*,#4416,.T.);
#5570=ORIENTED_EDGE('',*,*,#4417,.T.);
#5571=ORIENTED_EDGE('',*,*,#4405,.F.);
#5572=ORIENTED_EDGE('',*,*,#4418,.F.);
#5573=ORIENTED_EDGE('',*,*,#4419,.T.);
#5574=ORIENTED_EDGE('',*,*,#4418,.T.);
#5575=ORIENTED_EDGE('',*,*,#4404,.F.);
#5576=ORIENTED_EDGE('',*,*,#4395,.F.);
#5577=ORIENTED_EDGE('',*,*,#4399,.T.);
#5578=ORIENTED_EDGE('',*,*,#4407,.F.);
#5579=ORIENTED_EDGE('',*,*,#4386,.F.);
#5580=ORIENTED_EDGE('',*,*,#4390,.T.);
#5581=ORIENTED_EDGE('',*,*,#4411,.F.);
#5582=ORIENTED_EDGE('',*,*,#4420,.F.);
#5583=ORIENTED_EDGE('',*,*,#4421,.T.);
#5584=ORIENTED_EDGE('',*,*,#4420,.T.);
#5585=ORIENTED_EDGE('',*,*,#4410,.F.);
#5586=ORIENTED_EDGE('',*,*,#4422,.F.);
#5587=ORIENTED_EDGE('',*,*,#4423,.T.);
#5588=ORIENTED_EDGE('',*,*,#4422,.T.);
#5589=ORIENTED_EDGE('',*,*,#4409,.F.);
#5590=ORIENTED_EDGE('',*,*,#4392,.F.);
#5591=ORIENTED_EDGE('',*,*,#4388,.T.);
#5592=ORIENTED_EDGE('',*,*,#4408,.F.);
#5593=ORIENTED_EDGE('',*,*,#4401,.F.);
#5594=ORIENTED_EDGE('',*,*,#4397,.T.);
#5595=ORIENTED_EDGE('',*,*,#4406,.F.);
#5596=ORIENTED_EDGE('',*,*,#4417,.F.);
#5597=ORIENTED_EDGE('',*,*,#4423,.F.);
#5598=ORIENTED_EDGE('',*,*,#4416,.F.);
#5599=ORIENTED_EDGE('',*,*,#4419,.F.);
#5600=ORIENTED_EDGE('',*,*,#4421,.F.);
#5601=ORIENTED_EDGE('',*,*,#4412,.T.);
#5602=ORIENTED_EDGE('',*,*,#4414,.T.);
#5603=ORIENTED_EDGE('',*,*,#4424,.T.);
#5604=ORIENTED_EDGE('',*,*,#4425,.T.);
#5605=ORIENTED_EDGE('',*,*,#4426,.F.);
#5606=ORIENTED_EDGE('',*,*,#4427,.F.);
#5607=ORIENTED_EDGE('',*,*,#4428,.T.);
#5608=ORIENTED_EDGE('',*,*,#4427,.T.);
#5609=ORIENTED_EDGE('',*,*,#4429,.F.);
#5610=ORIENTED_EDGE('',*,*,#4430,.F.);
#5611=ORIENTED_EDGE('',*,*,#4431,.T.);
#5612=ORIENTED_EDGE('',*,*,#4430,.T.);
#5613=ORIENTED_EDGE('',*,*,#4432,.F.);
#5614=ORIENTED_EDGE('',*,*,#4433,.F.);
#5615=ORIENTED_EDGE('',*,*,#4434,.T.);
#5616=ORIENTED_EDGE('',*,*,#4433,.T.);
#5617=ORIENTED_EDGE('',*,*,#4435,.F.);
#5618=ORIENTED_EDGE('',*,*,#4425,.F.);
#5619=ORIENTED_EDGE('',*,*,#4435,.T.);
#5620=ORIENTED_EDGE('',*,*,#4432,.T.);
#5621=ORIENTED_EDGE('',*,*,#4429,.T.);
#5622=ORIENTED_EDGE('',*,*,#4426,.T.);
#5623=ORIENTED_EDGE('',*,*,#4434,.F.);
#5624=ORIENTED_EDGE('',*,*,#4424,.F.);
#5625=ORIENTED_EDGE('',*,*,#4428,.F.);
#5626=ORIENTED_EDGE('',*,*,#4431,.F.);
#5627=ORIENTED_EDGE('',*,*,#4436,.F.);
#5628=ORIENTED_EDGE('',*,*,#4437,.T.);
#5629=ORIENTED_EDGE('',*,*,#4438,.F.);
#5630=ORIENTED_EDGE('',*,*,#4439,.F.);
#5631=ORIENTED_EDGE('',*,*,#4440,.F.);
#5632=ORIENTED_EDGE('',*,*,#4441,.T.);
#5633=ORIENTED_EDGE('',*,*,#4442,.F.);
#5634=ORIENTED_EDGE('',*,*,#4437,.F.);
#5635=ORIENTED_EDGE('',*,*,#4443,.F.);
#5636=ORIENTED_EDGE('',*,*,#4444,.T.);
#5637=ORIENTED_EDGE('',*,*,#4445,.F.);
#5638=ORIENTED_EDGE('',*,*,#4441,.F.);
#5639=ORIENTED_EDGE('',*,*,#4446,.F.);
#5640=ORIENTED_EDGE('',*,*,#4447,.T.);
#5641=ORIENTED_EDGE('',*,*,#4448,.F.);
#5642=ORIENTED_EDGE('',*,*,#4444,.F.);
#5643=ORIENTED_EDGE('',*,*,#4449,.F.);
#5644=ORIENTED_EDGE('',*,*,#4450,.T.);
#5645=ORIENTED_EDGE('',*,*,#4451,.F.);
#5646=ORIENTED_EDGE('',*,*,#4447,.F.);
#5647=ORIENTED_EDGE('',*,*,#4452,.F.);
#5648=ORIENTED_EDGE('',*,*,#4453,.T.);
#5649=ORIENTED_EDGE('',*,*,#4454,.F.);
#5650=ORIENTED_EDGE('',*,*,#4450,.F.);
#5651=ORIENTED_EDGE('',*,*,#4455,.F.);
#5652=ORIENTED_EDGE('',*,*,#4456,.T.);
#5653=ORIENTED_EDGE('',*,*,#4457,.F.);
#5654=ORIENTED_EDGE('',*,*,#4453,.F.);
#5655=ORIENTED_EDGE('',*,*,#4458,.F.);
#5656=ORIENTED_EDGE('',*,*,#4459,.T.);
#5657=ORIENTED_EDGE('',*,*,#4460,.F.);
#5658=ORIENTED_EDGE('',*,*,#4456,.F.);
#5659=ORIENTED_EDGE('',*,*,#4461,.F.);
#5660=ORIENTED_EDGE('',*,*,#4462,.F.);
#5661=ORIENTED_EDGE('',*,*,#4463,.F.);
#5662=ORIENTED_EDGE('',*,*,#4459,.F.);
#5663=ORIENTED_EDGE('',*,*,#4464,.F.);
#5664=ORIENTED_EDGE('',*,*,#4465,.T.);
#5665=ORIENTED_EDGE('',*,*,#4466,.F.);
#5666=ORIENTED_EDGE('',*,*,#4467,.F.);
#5667=ORIENTED_EDGE('',*,*,#4468,.F.);
#5668=ORIENTED_EDGE('',*,*,#4469,.T.);
#5669=ORIENTED_EDGE('',*,*,#4470,.F.);
#5670=ORIENTED_EDGE('',*,*,#4465,.F.);
#5671=ORIENTED_EDGE('',*,*,#4471,.F.);
#5672=ORIENTED_EDGE('',*,*,#4472,.T.);
#5673=ORIENTED_EDGE('',*,*,#4473,.F.);
#5674=ORIENTED_EDGE('',*,*,#4469,.F.);
#5675=ORIENTED_EDGE('',*,*,#4474,.F.);
#5676=ORIENTED_EDGE('',*,*,#4475,.T.);
#5677=ORIENTED_EDGE('',*,*,#4476,.F.);
#5678=ORIENTED_EDGE('',*,*,#4472,.F.);
#5679=ORIENTED_EDGE('',*,*,#4477,.F.);
#5680=ORIENTED_EDGE('',*,*,#4478,.T.);
#5681=ORIENTED_EDGE('',*,*,#4479,.F.);
#5682=ORIENTED_EDGE('',*,*,#4475,.F.);
#5683=ORIENTED_EDGE('',*,*,#4480,.F.);
#5684=ORIENTED_EDGE('',*,*,#4481,.T.);
#5685=ORIENTED_EDGE('',*,*,#4482,.F.);
#5686=ORIENTED_EDGE('',*,*,#4478,.F.);
#5687=ORIENTED_EDGE('',*,*,#4483,.F.);
#5688=ORIENTED_EDGE('',*,*,#4484,.T.);
#5689=ORIENTED_EDGE('',*,*,#4485,.F.);
#5690=ORIENTED_EDGE('',*,*,#4481,.F.);
#5691=ORIENTED_EDGE('',*,*,#4486,.F.);
#5692=ORIENTED_EDGE('',*,*,#4487,.T.);
#5693=ORIENTED_EDGE('',*,*,#4488,.F.);
#5694=ORIENTED_EDGE('',*,*,#4484,.F.);
#5695=ORIENTED_EDGE('',*,*,#4489,.F.);
#5696=ORIENTED_EDGE('',*,*,#4490,.F.);
#5697=ORIENTED_EDGE('',*,*,#4491,.F.);
#5698=ORIENTED_EDGE('',*,*,#4487,.F.);
#5699=ORIENTED_EDGE('',*,*,#4492,.F.);
#5700=ORIENTED_EDGE('',*,*,#4493,.T.);
#5701=ORIENTED_EDGE('',*,*,#4494,.F.);
#5702=ORIENTED_EDGE('',*,*,#4495,.F.);
#5703=ORIENTED_EDGE('',*,*,#4496,.F.);
#5704=ORIENTED_EDGE('',*,*,#4497,.T.);
#5705=ORIENTED_EDGE('',*,*,#4498,.F.);
#5706=ORIENTED_EDGE('',*,*,#4493,.F.);
#5707=ORIENTED_EDGE('',*,*,#4499,.F.);
#5708=ORIENTED_EDGE('',*,*,#4500,.T.);
#5709=ORIENTED_EDGE('',*,*,#4501,.F.);
#5710=ORIENTED_EDGE('',*,*,#4497,.F.);
#5711=ORIENTED_EDGE('',*,*,#4502,.F.);
#5712=ORIENTED_EDGE('',*,*,#4503,.T.);
#5713=ORIENTED_EDGE('',*,*,#4504,.F.);
#5714=ORIENTED_EDGE('',*,*,#4500,.F.);
#5715=ORIENTED_EDGE('',*,*,#4505,.F.);
#5716=ORIENTED_EDGE('',*,*,#4506,.T.);
#5717=ORIENTED_EDGE('',*,*,#4507,.F.);
#5718=ORIENTED_EDGE('',*,*,#4503,.F.);
#5719=ORIENTED_EDGE('',*,*,#4508,.F.);
#5720=ORIENTED_EDGE('',*,*,#4509,.T.);
#5721=ORIENTED_EDGE('',*,*,#4510,.F.);
#5722=ORIENTED_EDGE('',*,*,#4506,.F.);
#5723=ORIENTED_EDGE('',*,*,#4511,.F.);
#5724=ORIENTED_EDGE('',*,*,#4512,.T.);
#5725=ORIENTED_EDGE('',*,*,#4513,.F.);
#5726=ORIENTED_EDGE('',*,*,#4509,.F.);
#5727=ORIENTED_EDGE('',*,*,#4514,.F.);
#5728=ORIENTED_EDGE('',*,*,#4515,.T.);
#5729=ORIENTED_EDGE('',*,*,#4516,.F.);
#5730=ORIENTED_EDGE('',*,*,#4512,.F.);
#5731=ORIENTED_EDGE('',*,*,#4517,.F.);
#5732=ORIENTED_EDGE('',*,*,#4518,.F.);
#5733=ORIENTED_EDGE('',*,*,#4519,.F.);
#5734=ORIENTED_EDGE('',*,*,#4515,.F.);
#5735=ORIENTED_EDGE('',*,*,#4520,.F.);
#5736=ORIENTED_EDGE('',*,*,#4521,.T.);
#5737=ORIENTED_EDGE('',*,*,#4522,.F.);
#5738=ORIENTED_EDGE('',*,*,#4523,.F.);
#5739=ORIENTED_EDGE('',*,*,#4524,.F.);
#5740=ORIENTED_EDGE('',*,*,#4525,.T.);
#5741=ORIENTED_EDGE('',*,*,#4526,.F.);
#5742=ORIENTED_EDGE('',*,*,#4521,.F.);
#5743=ORIENTED_EDGE('',*,*,#4527,.F.);
#5744=ORIENTED_EDGE('',*,*,#4528,.T.);
#5745=ORIENTED_EDGE('',*,*,#4529,.F.);
#5746=ORIENTED_EDGE('',*,*,#4525,.F.);
#5747=ORIENTED_EDGE('',*,*,#4530,.F.);
#5748=ORIENTED_EDGE('',*,*,#4531,.T.);
#5749=ORIENTED_EDGE('',*,*,#4532,.F.);
#5750=ORIENTED_EDGE('',*,*,#4528,.F.);
#5751=ORIENTED_EDGE('',*,*,#4533,.F.);
#5752=ORIENTED_EDGE('',*,*,#4534,.T.);
#5753=ORIENTED_EDGE('',*,*,#4535,.F.);
#5754=ORIENTED_EDGE('',*,*,#4531,.F.);
#5755=ORIENTED_EDGE('',*,*,#4536,.F.);
#5756=ORIENTED_EDGE('',*,*,#4537,.T.);
#5757=ORIENTED_EDGE('',*,*,#4538,.F.);
#5758=ORIENTED_EDGE('',*,*,#4534,.F.);
#5759=ORIENTED_EDGE('',*,*,#4539,.F.);
#5760=ORIENTED_EDGE('',*,*,#4540,.T.);
#5761=ORIENTED_EDGE('',*,*,#4541,.F.);
#5762=ORIENTED_EDGE('',*,*,#4537,.F.);
#5763=ORIENTED_EDGE('',*,*,#4542,.F.);
#5764=ORIENTED_EDGE('',*,*,#4543,.T.);
#5765=ORIENTED_EDGE('',*,*,#4544,.F.);
#5766=ORIENTED_EDGE('',*,*,#4540,.F.);
#5767=ORIENTED_EDGE('',*,*,#4545,.F.);
#5768=ORIENTED_EDGE('',*,*,#4546,.F.);
#5769=ORIENTED_EDGE('',*,*,#4547,.F.);
#5770=ORIENTED_EDGE('',*,*,#4543,.F.);
#5771=ORIENTED_EDGE('',*,*,#4548,.F.);
#5772=ORIENTED_EDGE('',*,*,#4549,.T.);
#5773=ORIENTED_EDGE('',*,*,#4550,.F.);
#5774=ORIENTED_EDGE('',*,*,#4549,.F.);
#5775=ORIENTED_EDGE('',*,*,#4462,.T.);
#5776=ORIENTED_EDGE('',*,*,#4551,.T.);
#5777=ORIENTED_EDGE('',*,*,#4552,.T.);
#5778=ORIENTED_EDGE('',*,*,#4553,.F.);
#5779=ORIENTED_EDGE('',*,*,#4439,.T.);
#5780=ORIENTED_EDGE('',*,*,#4554,.F.);
#5781=ORIENTED_EDGE('',*,*,#4555,.F.);
#5782=ORIENTED_EDGE('',*,*,#4556,.T.);
#5783=ORIENTED_EDGE('',*,*,#4490,.T.);
#5784=ORIENTED_EDGE('',*,*,#4557,.T.);
#5785=ORIENTED_EDGE('',*,*,#4555,.T.);
#5786=ORIENTED_EDGE('',*,*,#4558,.F.);
#5787=ORIENTED_EDGE('',*,*,#4467,.T.);
#5788=ORIENTED_EDGE('',*,*,#4559,.F.);
#5789=ORIENTED_EDGE('',*,*,#4560,.F.);
#5790=ORIENTED_EDGE('',*,*,#4561,.T.);
#5791=ORIENTED_EDGE('',*,*,#4518,.T.);
#5792=ORIENTED_EDGE('',*,*,#4562,.T.);
#5793=ORIENTED_EDGE('',*,*,#4560,.T.);
#5794=ORIENTED_EDGE('',*,*,#4563,.F.);
#5795=ORIENTED_EDGE('',*,*,#4495,.T.);
#5796=ORIENTED_EDGE('',*,*,#4564,.F.);
#5797=ORIENTED_EDGE('',*,*,#4565,.F.);
#5798=ORIENTED_EDGE('',*,*,#4566,.T.);
#5799=ORIENTED_EDGE('',*,*,#4546,.T.);
#5800=ORIENTED_EDGE('',*,*,#4567,.T.);
#5801=ORIENTED_EDGE('',*,*,#4565,.T.);
#5802=ORIENTED_EDGE('',*,*,#4568,.F.);
#5803=ORIENTED_EDGE('',*,*,#4523,.T.);
#5804=ORIENTED_EDGE('',*,*,#4569,.F.);
#5805=ORIENTED_EDGE('',*,*,#4552,.F.);
#5806=ORIENTED_EDGE('',*,*,#4570,.T.);
#5807=ORIENTED_EDGE('',*,*,#4438,.T.);
#5808=ORIENTED_EDGE('',*,*,#4442,.T.);
#5809=ORIENTED_EDGE('',*,*,#4445,.T.);
#5810=ORIENTED_EDGE('',*,*,#4448,.T.);
#5811=ORIENTED_EDGE('',*,*,#4451,.T.);
#5812=ORIENTED_EDGE('',*,*,#4454,.T.);
#5813=ORIENTED_EDGE('',*,*,#4457,.T.);
#5814=ORIENTED_EDGE('',*,*,#4460,.T.);
#5815=ORIENTED_EDGE('',*,*,#4463,.T.);
#5816=ORIENTED_EDGE('',*,*,#4553,.T.);
#5817=ORIENTED_EDGE('',*,*,#4569,.T.);
#5818=ORIENTED_EDGE('',*,*,#4522,.T.);
#5819=ORIENTED_EDGE('',*,*,#4526,.T.);
#5820=ORIENTED_EDGE('',*,*,#4529,.T.);
#5821=ORIENTED_EDGE('',*,*,#4532,.T.);
#5822=ORIENTED_EDGE('',*,*,#4535,.T.);
#5823=ORIENTED_EDGE('',*,*,#4538,.T.);
#5824=ORIENTED_EDGE('',*,*,#4541,.T.);
#5825=ORIENTED_EDGE('',*,*,#4544,.T.);
#5826=ORIENTED_EDGE('',*,*,#4547,.T.);
#5827=ORIENTED_EDGE('',*,*,#4568,.T.);
#5828=ORIENTED_EDGE('',*,*,#4564,.T.);
#5829=ORIENTED_EDGE('',*,*,#4494,.T.);
#5830=ORIENTED_EDGE('',*,*,#4498,.T.);
#5831=ORIENTED_EDGE('',*,*,#4501,.T.);
#5832=ORIENTED_EDGE('',*,*,#4504,.T.);
#5833=ORIENTED_EDGE('',*,*,#4507,.T.);
#5834=ORIENTED_EDGE('',*,*,#4510,.T.);
#5835=ORIENTED_EDGE('',*,*,#4513,.T.);
#5836=ORIENTED_EDGE('',*,*,#4516,.T.);
#5837=ORIENTED_EDGE('',*,*,#4519,.T.);
#5838=ORIENTED_EDGE('',*,*,#4563,.T.);
#5839=ORIENTED_EDGE('',*,*,#4559,.T.);
#5840=ORIENTED_EDGE('',*,*,#4466,.T.);
#5841=ORIENTED_EDGE('',*,*,#4470,.T.);
#5842=ORIENTED_EDGE('',*,*,#4473,.T.);
#5843=ORIENTED_EDGE('',*,*,#4476,.T.);
#5844=ORIENTED_EDGE('',*,*,#4479,.T.);
#5845=ORIENTED_EDGE('',*,*,#4482,.T.);
#5846=ORIENTED_EDGE('',*,*,#4485,.T.);
#5847=ORIENTED_EDGE('',*,*,#4488,.T.);
#5848=ORIENTED_EDGE('',*,*,#4491,.T.);
#5849=ORIENTED_EDGE('',*,*,#4558,.T.);
#5850=ORIENTED_EDGE('',*,*,#4554,.T.);
#5851=ORIENTED_EDGE('',*,*,#4550,.T.);
#5852=ORIENTED_EDGE('',*,*,#4436,.T.);
#5853=ORIENTED_EDGE('',*,*,#4556,.F.);
#5854=ORIENTED_EDGE('',*,*,#4557,.F.);
#5855=ORIENTED_EDGE('',*,*,#4489,.T.);
#5856=ORIENTED_EDGE('',*,*,#4486,.T.);
#5857=ORIENTED_EDGE('',*,*,#4483,.T.);
#5858=ORIENTED_EDGE('',*,*,#4480,.T.);
#5859=ORIENTED_EDGE('',*,*,#4477,.T.);
#5860=ORIENTED_EDGE('',*,*,#4474,.T.);
#5861=ORIENTED_EDGE('',*,*,#4471,.T.);
#5862=ORIENTED_EDGE('',*,*,#4468,.T.);
#5863=ORIENTED_EDGE('',*,*,#4464,.T.);
#5864=ORIENTED_EDGE('',*,*,#4561,.F.);
#5865=ORIENTED_EDGE('',*,*,#4562,.F.);
#5866=ORIENTED_EDGE('',*,*,#4517,.T.);
#5867=ORIENTED_EDGE('',*,*,#4514,.T.);
#5868=ORIENTED_EDGE('',*,*,#4511,.T.);
#5869=ORIENTED_EDGE('',*,*,#4508,.T.);
#5870=ORIENTED_EDGE('',*,*,#4505,.T.);
#5871=ORIENTED_EDGE('',*,*,#4502,.T.);
#5872=ORIENTED_EDGE('',*,*,#4499,.T.);
#5873=ORIENTED_EDGE('',*,*,#4496,.T.);
#5874=ORIENTED_EDGE('',*,*,#4492,.T.);
#5875=ORIENTED_EDGE('',*,*,#4566,.F.);
#5876=ORIENTED_EDGE('',*,*,#4567,.F.);
#5877=ORIENTED_EDGE('',*,*,#4545,.T.);
#5878=ORIENTED_EDGE('',*,*,#4542,.T.);
#5879=ORIENTED_EDGE('',*,*,#4539,.T.);
#5880=ORIENTED_EDGE('',*,*,#4536,.T.);
#5881=ORIENTED_EDGE('',*,*,#4533,.T.);
#5882=ORIENTED_EDGE('',*,*,#4530,.T.);
#5883=ORIENTED_EDGE('',*,*,#4527,.T.);
#5884=ORIENTED_EDGE('',*,*,#4524,.T.);
#5885=ORIENTED_EDGE('',*,*,#4520,.T.);
#5886=ORIENTED_EDGE('',*,*,#4570,.F.);
#5887=ORIENTED_EDGE('',*,*,#4551,.F.);
#5888=ORIENTED_EDGE('',*,*,#4461,.T.);
#5889=ORIENTED_EDGE('',*,*,#4458,.T.);
#5890=ORIENTED_EDGE('',*,*,#4455,.T.);
#5891=ORIENTED_EDGE('',*,*,#4452,.T.);
#5892=ORIENTED_EDGE('',*,*,#4449,.T.);
#5893=ORIENTED_EDGE('',*,*,#4446,.T.);
#5894=ORIENTED_EDGE('',*,*,#4443,.T.);
#5895=ORIENTED_EDGE('',*,*,#4440,.T.);
#5896=ORIENTED_EDGE('',*,*,#4548,.T.);
#5897=ORIENTED_EDGE('',*,*,#4571,.F.);
#5898=ORIENTED_EDGE('',*,*,#4572,.T.);
#5899=ORIENTED_EDGE('',*,*,#4573,.F.);
#5900=ORIENTED_EDGE('',*,*,#4572,.F.);
#5901=ORIENTED_EDGE('',*,*,#4571,.T.);
#5902=ORIENTED_EDGE('',*,*,#4574,.F.);
#5903=ORIENTED_EDGE('',*,*,#4575,.F.);
#5904=ORIENTED_EDGE('',*,*,#4576,.T.);
#5905=ORIENTED_EDGE('',*,*,#4577,.F.);
#5906=ORIENTED_EDGE('',*,*,#4576,.F.);
#5907=ORIENTED_EDGE('',*,*,#4575,.T.);
#5908=ORIENTED_EDGE('',*,*,#4578,.F.);
#5909=ORIENTED_EDGE('',*,*,#4579,.F.);
#5910=ORIENTED_EDGE('',*,*,#4580,.T.);
#5911=ORIENTED_EDGE('',*,*,#4581,.F.);
#5912=ORIENTED_EDGE('',*,*,#4580,.F.);
#5913=ORIENTED_EDGE('',*,*,#4579,.T.);
#5914=ORIENTED_EDGE('',*,*,#4582,.F.);
#5915=ORIENTED_EDGE('',*,*,#4583,.F.);
#5916=ORIENTED_EDGE('',*,*,#4584,.T.);
#5917=ORIENTED_EDGE('',*,*,#4585,.F.);
#5918=ORIENTED_EDGE('',*,*,#4584,.F.);
#5919=ORIENTED_EDGE('',*,*,#4583,.T.);
#5920=ORIENTED_EDGE('',*,*,#4586,.F.);
#5921=ORIENTED_EDGE('',*,*,#4587,.F.);
#5922=ORIENTED_EDGE('',*,*,#4588,.T.);
#5923=ORIENTED_EDGE('',*,*,#4574,.T.);
#5924=ORIENTED_EDGE('',*,*,#4588,.F.);
#5925=ORIENTED_EDGE('',*,*,#4589,.F.);
#5926=ORIENTED_EDGE('',*,*,#4590,.T.);
#5927=ORIENTED_EDGE('',*,*,#4578,.T.);
#5928=ORIENTED_EDGE('',*,*,#4590,.F.);
#5929=ORIENTED_EDGE('',*,*,#4591,.F.);
#5930=ORIENTED_EDGE('',*,*,#4592,.T.);
#5931=ORIENTED_EDGE('',*,*,#4582,.T.);
#5932=ORIENTED_EDGE('',*,*,#4592,.F.);
#5933=ORIENTED_EDGE('',*,*,#4593,.F.);
#5934=ORIENTED_EDGE('',*,*,#4594,.T.);
#5935=ORIENTED_EDGE('',*,*,#4586,.T.);
#5936=ORIENTED_EDGE('',*,*,#4594,.F.);
#5937=ORIENTED_EDGE('',*,*,#4595,.T.);
#5938=ORIENTED_EDGE('',*,*,#4596,.T.);
#5939=ORIENTED_EDGE('',*,*,#4597,.F.);
#5940=ORIENTED_EDGE('',*,*,#4598,.F.);
#5941=ORIENTED_EDGE('',*,*,#4599,.T.);
#5942=ORIENTED_EDGE('',*,*,#4598,.T.);
#5943=ORIENTED_EDGE('',*,*,#4600,.F.);
#5944=ORIENTED_EDGE('',*,*,#4601,.F.);
#5945=ORIENTED_EDGE('',*,*,#4602,.T.);
#5946=ORIENTED_EDGE('',*,*,#4601,.T.);
#5947=ORIENTED_EDGE('',*,*,#4603,.F.);
#5948=ORIENTED_EDGE('',*,*,#4604,.F.);
#5949=ORIENTED_EDGE('',*,*,#4605,.T.);
#5950=ORIENTED_EDGE('',*,*,#4604,.T.);
#5951=ORIENTED_EDGE('',*,*,#4606,.F.);
#5952=ORIENTED_EDGE('',*,*,#4607,.F.);
#5953=ORIENTED_EDGE('',*,*,#4608,.T.);
#5954=ORIENTED_EDGE('',*,*,#4607,.T.);
#5955=ORIENTED_EDGE('',*,*,#4609,.F.);
#5956=ORIENTED_EDGE('',*,*,#4610,.F.);
#5957=ORIENTED_EDGE('',*,*,#4585,.T.);
#5958=ORIENTED_EDGE('',*,*,#4581,.T.);
#5959=ORIENTED_EDGE('',*,*,#4577,.T.);
#5960=ORIENTED_EDGE('',*,*,#4573,.T.);
#5961=ORIENTED_EDGE('',*,*,#4611,.T.);
#5962=ORIENTED_EDGE('',*,*,#4610,.T.);
#5963=ORIENTED_EDGE('',*,*,#4612,.F.);
#5964=ORIENTED_EDGE('',*,*,#4613,.F.);
#5965=ORIENTED_EDGE('',*,*,#4614,.T.);
#5966=ORIENTED_EDGE('',*,*,#4613,.T.);
#5967=ORIENTED_EDGE('',*,*,#4615,.F.);
#5968=ORIENTED_EDGE('',*,*,#4616,.F.);
#5969=ORIENTED_EDGE('',*,*,#4617,.T.);
#5970=ORIENTED_EDGE('',*,*,#4616,.T.);
#5971=ORIENTED_EDGE('',*,*,#4618,.F.);
#5972=ORIENTED_EDGE('',*,*,#4619,.F.);
#5973=ORIENTED_EDGE('',*,*,#4620,.T.);
#5974=ORIENTED_EDGE('',*,*,#4619,.T.);
#5975=ORIENTED_EDGE('',*,*,#4621,.F.);
#5976=ORIENTED_EDGE('',*,*,#4622,.F.);
#5977=ORIENTED_EDGE('',*,*,#4623,.T.);
#5978=ORIENTED_EDGE('',*,*,#4622,.T.);
#5979=ORIENTED_EDGE('',*,*,#4624,.F.);
#5980=ORIENTED_EDGE('',*,*,#4625,.F.);
#5981=ORIENTED_EDGE('',*,*,#4626,.T.);
#5982=ORIENTED_EDGE('',*,*,#4625,.T.);
#5983=ORIENTED_EDGE('',*,*,#4627,.F.);
#5984=ORIENTED_EDGE('',*,*,#4628,.F.);
#5985=ORIENTED_EDGE('',*,*,#4587,.T.);
#5986=ORIENTED_EDGE('',*,*,#4589,.T.);
#5987=ORIENTED_EDGE('',*,*,#4591,.T.);
#5988=ORIENTED_EDGE('',*,*,#4593,.T.);
#5989=ORIENTED_EDGE('',*,*,#4629,.T.);
#5990=ORIENTED_EDGE('',*,*,#4628,.T.);
#5991=ORIENTED_EDGE('',*,*,#4630,.F.);
#5992=ORIENTED_EDGE('',*,*,#4596,.F.);
#5993=ORIENTED_EDGE('',*,*,#4630,.T.);
#5994=ORIENTED_EDGE('',*,*,#4627,.T.);
#5995=ORIENTED_EDGE('',*,*,#4624,.T.);
#5996=ORIENTED_EDGE('',*,*,#4621,.T.);
#5997=ORIENTED_EDGE('',*,*,#4618,.T.);
#5998=ORIENTED_EDGE('',*,*,#4615,.T.);
#5999=ORIENTED_EDGE('',*,*,#4612,.T.);
#6000=ORIENTED_EDGE('',*,*,#4609,.T.);
#6001=ORIENTED_EDGE('',*,*,#4606,.T.);
#6002=ORIENTED_EDGE('',*,*,#4603,.T.);
#6003=ORIENTED_EDGE('',*,*,#4600,.T.);
#6004=ORIENTED_EDGE('',*,*,#4597,.T.);
#6005=ORIENTED_EDGE('',*,*,#4629,.F.);
#6006=ORIENTED_EDGE('',*,*,#4595,.F.);
#6007=ORIENTED_EDGE('',*,*,#4599,.F.);
#6008=ORIENTED_EDGE('',*,*,#4602,.F.);
#6009=ORIENTED_EDGE('',*,*,#4605,.F.);
#6010=ORIENTED_EDGE('',*,*,#4608,.F.);
#6011=ORIENTED_EDGE('',*,*,#4611,.F.);
#6012=ORIENTED_EDGE('',*,*,#4614,.F.);
#6013=ORIENTED_EDGE('',*,*,#4617,.F.);
#6014=ORIENTED_EDGE('',*,*,#4620,.F.);
#6015=ORIENTED_EDGE('',*,*,#4623,.F.);
#6016=ORIENTED_EDGE('',*,*,#4626,.F.);
#6017=ORIENTED_EDGE('',*,*,#4631,.F.);
#6018=ORIENTED_EDGE('',*,*,#4632,.F.);
#6019=ORIENTED_EDGE('',*,*,#4633,.T.);
#6020=ORIENTED_EDGE('',*,*,#4631,.T.);
#6021=ORIENTED_EDGE('',*,*,#4633,.F.);
#6022=ORIENTED_EDGE('',*,*,#4634,.F.);
#6023=ORIENTED_EDGE('',*,*,#4635,.T.);
#6024=ORIENTED_EDGE('',*,*,#4632,.T.);
#6025=ORIENTED_EDGE('',*,*,#4635,.F.);
#6026=ORIENTED_EDGE('',*,*,#4636,.F.);
#6027=ORIENTED_EDGE('',*,*,#4637,.T.);
#6028=ORIENTED_EDGE('',*,*,#4634,.T.);
#6029=ORIENTED_EDGE('',*,*,#4637,.F.);
#6030=ORIENTED_EDGE('',*,*,#4636,.T.);
#6031=ORIENTED_EDGE('',*,*,#4638,.F.);
#6032=ORIENTED_EDGE('',*,*,#4639,.F.);
#6033=ORIENTED_EDGE('',*,*,#4640,.T.);
#6034=ORIENTED_EDGE('',*,*,#4638,.T.);
#6035=ORIENTED_EDGE('',*,*,#4640,.F.);
#6036=ORIENTED_EDGE('',*,*,#4641,.F.);
#6037=ORIENTED_EDGE('',*,*,#4642,.T.);
#6038=ORIENTED_EDGE('',*,*,#4639,.T.);
#6039=ORIENTED_EDGE('',*,*,#4642,.F.);
#6040=ORIENTED_EDGE('',*,*,#4643,.F.);
#6041=ORIENTED_EDGE('',*,*,#4644,.T.);
#6042=ORIENTED_EDGE('',*,*,#4641,.T.);
#6043=ORIENTED_EDGE('',*,*,#4644,.F.);
#6044=ORIENTED_EDGE('',*,*,#4643,.T.);
#6045=ORIENTED_EDGE('',*,*,#4645,.T.);
#6046=ORIENTED_EDGE('',*,*,#4646,.T.);
#6047=ORIENTED_EDGE('',*,*,#4647,.T.);
#6048=ORIENTED_EDGE('',*,*,#4648,.F.);
#6049=ORIENTED_EDGE('',*,*,#4649,.T.);
#6050=ORIENTED_EDGE('',*,*,#4650,.T.);
#6051=ORIENTED_EDGE('',*,*,#4651,.T.);
#6052=ORIENTED_EDGE('',*,*,#4646,.F.);
#6053=ORIENTED_EDGE('',*,*,#4652,.T.);
#6054=ORIENTED_EDGE('',*,*,#4653,.T.);
#6055=ORIENTED_EDGE('',*,*,#4654,.T.);
#6056=ORIENTED_EDGE('',*,*,#4650,.F.);
#6057=ORIENTED_EDGE('',*,*,#4655,.T.);
#6058=ORIENTED_EDGE('',*,*,#4656,.T.);
#6059=ORIENTED_EDGE('',*,*,#4657,.T.);
#6060=ORIENTED_EDGE('',*,*,#4653,.F.);
#6061=ORIENTED_EDGE('',*,*,#4658,.T.);
#6062=ORIENTED_EDGE('',*,*,#4659,.T.);
#6063=ORIENTED_EDGE('',*,*,#4660,.T.);
#6064=ORIENTED_EDGE('',*,*,#4656,.F.);
#6065=ORIENTED_EDGE('',*,*,#4661,.T.);
#6066=ORIENTED_EDGE('',*,*,#4648,.T.);
#6067=ORIENTED_EDGE('',*,*,#4662,.T.);
#6068=ORIENTED_EDGE('',*,*,#4659,.F.);
#6069=ORIENTED_EDGE('',*,*,#4661,.F.);
#6070=ORIENTED_EDGE('',*,*,#4658,.F.);
#6071=ORIENTED_EDGE('',*,*,#4655,.F.);
#6072=ORIENTED_EDGE('',*,*,#4652,.F.);
#6073=ORIENTED_EDGE('',*,*,#4649,.F.);
#6074=ORIENTED_EDGE('',*,*,#4645,.F.);
#6075=ORIENTED_EDGE('',*,*,#4662,.F.);
#6076=ORIENTED_EDGE('',*,*,#4647,.F.);
#6077=ORIENTED_EDGE('',*,*,#4651,.F.);
#6078=ORIENTED_EDGE('',*,*,#4654,.F.);
#6079=ORIENTED_EDGE('',*,*,#4657,.F.);
#6080=ORIENTED_EDGE('',*,*,#4660,.F.);
#6081=ORIENTED_EDGE('',*,*,#4663,.F.);
#6082=ORIENTED_EDGE('',*,*,#4664,.F.);
#6083=ORIENTED_EDGE('',*,*,#4665,.F.);
#6084=ORIENTED_EDGE('',*,*,#4666,.F.);
#6085=ORIENTED_EDGE('',*,*,#4665,.T.);
#6086=ORIENTED_EDGE('',*,*,#4667,.T.);
#6087=ORIENTED_EDGE('',*,*,#4668,.F.);
#6088=ORIENTED_EDGE('',*,*,#4669,.F.);
#6089=ORIENTED_EDGE('',*,*,#4670,.T.);
#6090=ORIENTED_EDGE('',*,*,#4671,.T.);
#6091=ORIENTED_EDGE('',*,*,#4672,.T.);
#6092=ORIENTED_EDGE('',*,*,#4668,.T.);
#6093=ORIENTED_EDGE('',*,*,#4673,.T.);
#6094=ORIENTED_EDGE('',*,*,#4670,.F.);
#6095=ORIENTED_EDGE('',*,*,#4667,.F.);
#6096=ORIENTED_EDGE('',*,*,#4664,.T.);
#6097=ORIENTED_EDGE('',*,*,#4674,.F.);
#6098=ORIENTED_EDGE('',*,*,#4675,.F.);
#6099=ORIENTED_EDGE('',*,*,#4676,.T.);
#6100=ORIENTED_EDGE('',*,*,#4677,.F.);
#6101=ORIENTED_EDGE('',*,*,#4678,.T.);
#6102=ORIENTED_EDGE('',*,*,#4679,.T.);
#6103=ORIENTED_EDGE('',*,*,#4680,.T.);
#6104=ORIENTED_EDGE('',*,*,#4681,.T.);
#6105=ORIENTED_EDGE('',*,*,#4682,.T.);
#6106=ORIENTED_EDGE('',*,*,#4671,.F.);
#6107=ORIENTED_EDGE('',*,*,#4680,.F.);
#6108=ORIENTED_EDGE('',*,*,#4683,.F.);
#6109=ORIENTED_EDGE('',*,*,#4684,.F.);
#6110=ORIENTED_EDGE('',*,*,#4681,.F.);
#6111=ORIENTED_EDGE('',*,*,#4679,.F.);
#6112=ORIENTED_EDGE('',*,*,#4672,.F.);
#6113=ORIENTED_EDGE('',*,*,#4682,.F.);
#6114=ORIENTED_EDGE('',*,*,#4684,.T.);
#6115=ORIENTED_EDGE('',*,*,#4685,.F.);
#6116=ORIENTED_EDGE('',*,*,#4686,.F.);
#6117=ORIENTED_EDGE('',*,*,#4687,.T.);
#6118=ORIENTED_EDGE('',*,*,#4688,.F.);
#6119=ORIENTED_EDGE('',*,*,#4689,.T.);
#6120=ORIENTED_EDGE('',*,*,#4666,.T.);
#6121=ORIENTED_EDGE('',*,*,#4669,.T.);
#6122=ORIENTED_EDGE('',*,*,#4683,.T.);
#6123=ORIENTED_EDGE('',*,*,#4678,.F.);
#6124=ORIENTED_EDGE('',*,*,#4690,.F.);
#6125=ORIENTED_EDGE('',*,*,#4685,.T.);
#6126=ORIENTED_EDGE('',*,*,#4686,.T.);
#6127=ORIENTED_EDGE('',*,*,#4690,.T.);
#6128=ORIENTED_EDGE('',*,*,#4677,.T.);
#6129=ORIENTED_EDGE('',*,*,#4691,.T.);
#6130=ORIENTED_EDGE('',*,*,#4692,.T.);
#6131=ORIENTED_EDGE('',*,*,#4693,.T.);
#6132=ORIENTED_EDGE('',*,*,#4692,.F.);
#6133=ORIENTED_EDGE('',*,*,#4694,.F.);
#6134=ORIENTED_EDGE('',*,*,#4695,.T.);
#6135=ORIENTED_EDGE('',*,*,#4673,.F.);
#6136=ORIENTED_EDGE('',*,*,#4695,.F.);
#6137=ORIENTED_EDGE('',*,*,#4696,.F.);
#6138=ORIENTED_EDGE('',*,*,#4697,.F.);
#6139=ORIENTED_EDGE('',*,*,#4698,.F.);
#6140=ORIENTED_EDGE('',*,*,#4691,.F.);
#6141=ORIENTED_EDGE('',*,*,#4676,.F.);
#6142=ORIENTED_EDGE('',*,*,#4699,.F.);
#6143=ORIENTED_EDGE('',*,*,#4696,.T.);
#6144=ORIENTED_EDGE('',*,*,#4694,.T.);
#6145=ORIENTED_EDGE('',*,*,#4693,.F.);
#6146=ORIENTED_EDGE('',*,*,#4698,.T.);
#6147=ORIENTED_EDGE('',*,*,#4700,.F.);
#6148=ORIENTED_EDGE('',*,*,#4687,.F.);
#6149=ORIENTED_EDGE('',*,*,#4675,.T.);
#6150=ORIENTED_EDGE('',*,*,#4701,.T.);
#6151=ORIENTED_EDGE('',*,*,#4688,.T.);
#6152=ORIENTED_EDGE('',*,*,#4700,.T.);
#6153=ORIENTED_EDGE('',*,*,#4697,.T.);
#6154=ORIENTED_EDGE('',*,*,#4699,.T.);
#6155=ORIENTED_EDGE('',*,*,#4663,.T.);
#6156=ORIENTED_EDGE('',*,*,#4689,.F.);
#6157=ORIENTED_EDGE('',*,*,#4701,.F.);
#6158=ORIENTED_EDGE('',*,*,#4674,.T.);
#6159=ORIENTED_EDGE('',*,*,#4702,.T.);
#6160=ORIENTED_EDGE('',*,*,#4703,.T.);
#6161=ORIENTED_EDGE('',*,*,#4704,.T.);
#6162=ORIENTED_EDGE('',*,*,#4705,.F.);
#6163=ORIENTED_EDGE('',*,*,#4706,.T.);
#6164=ORIENTED_EDGE('',*,*,#4707,.T.);
#6165=ORIENTED_EDGE('',*,*,#4708,.T.);
#6166=ORIENTED_EDGE('',*,*,#4703,.F.);
#6167=ORIENTED_EDGE('',*,*,#4709,.T.);
#6168=ORIENTED_EDGE('',*,*,#4710,.T.);
#6169=ORIENTED_EDGE('',*,*,#4711,.T.);
#6170=ORIENTED_EDGE('',*,*,#4707,.F.);
#6171=ORIENTED_EDGE('',*,*,#4712,.T.);
#6172=ORIENTED_EDGE('',*,*,#4713,.T.);
#6173=ORIENTED_EDGE('',*,*,#4714,.T.);
#6174=ORIENTED_EDGE('',*,*,#4710,.F.);
#6175=ORIENTED_EDGE('',*,*,#4715,.T.);
#6176=ORIENTED_EDGE('',*,*,#4716,.T.);
#6177=ORIENTED_EDGE('',*,*,#4717,.T.);
#6178=ORIENTED_EDGE('',*,*,#4713,.F.);
#6179=ORIENTED_EDGE('',*,*,#4718,.T.);
#6180=ORIENTED_EDGE('',*,*,#4705,.T.);
#6181=ORIENTED_EDGE('',*,*,#4719,.T.);
#6182=ORIENTED_EDGE('',*,*,#4716,.F.);
#6183=ORIENTED_EDGE('',*,*,#4718,.F.);
#6184=ORIENTED_EDGE('',*,*,#4715,.F.);
#6185=ORIENTED_EDGE('',*,*,#4712,.F.);
#6186=ORIENTED_EDGE('',*,*,#4709,.F.);
#6187=ORIENTED_EDGE('',*,*,#4706,.F.);
#6188=ORIENTED_EDGE('',*,*,#4702,.F.);
#6189=ORIENTED_EDGE('',*,*,#4719,.F.);
#6190=ORIENTED_EDGE('',*,*,#4704,.F.);
#6191=ORIENTED_EDGE('',*,*,#4708,.F.);
#6192=ORIENTED_EDGE('',*,*,#4711,.F.);
#6193=ORIENTED_EDGE('',*,*,#4714,.F.);
#6194=ORIENTED_EDGE('',*,*,#4717,.F.);
#6195=ORIENTED_EDGE('',*,*,#4720,.F.);
#6196=ORIENTED_EDGE('',*,*,#4721,.F.);
#6197=ORIENTED_EDGE('',*,*,#4722,.F.);
#6198=ORIENTED_EDGE('',*,*,#4723,.T.);
#6199=ORIENTED_EDGE('',*,*,#4721,.T.);
#6200=ORIENTED_EDGE('',*,*,#4723,.F.);
#6201=ORIENTED_EDGE('',*,*,#4724,.F.);
#6202=ORIENTED_EDGE('',*,*,#4725,.T.);
#6203=ORIENTED_EDGE('',*,*,#4722,.T.);
#6204=ORIENTED_EDGE('',*,*,#4725,.F.);
#6205=ORIENTED_EDGE('',*,*,#4726,.F.);
#6206=ORIENTED_EDGE('',*,*,#4727,.T.);
#6207=ORIENTED_EDGE('',*,*,#4724,.T.);
#6208=ORIENTED_EDGE('',*,*,#4727,.F.);
#6209=ORIENTED_EDGE('',*,*,#4726,.T.);
#6210=ORIENTED_EDGE('',*,*,#4728,.F.);
#6211=ORIENTED_EDGE('',*,*,#4729,.F.);
#6212=ORIENTED_EDGE('',*,*,#4730,.T.);
#6213=ORIENTED_EDGE('',*,*,#4728,.T.);
#6214=ORIENTED_EDGE('',*,*,#4730,.F.);
#6215=ORIENTED_EDGE('',*,*,#4720,.T.);
#6216=ORIENTED_EDGE('',*,*,#4731,.T.);
#6217=ORIENTED_EDGE('',*,*,#4729,.T.);
#6218=ORIENTED_EDGE('',*,*,#4731,.F.);
#6219=ORIENTED_EDGE('',*,*,#4732,.F.);
#6220=ORIENTED_EDGE('',*,*,#4733,.T.);
#6221=ORIENTED_EDGE('',*,*,#4734,.F.);
#6222=ORIENTED_EDGE('',*,*,#4733,.F.);
#6223=ORIENTED_EDGE('',*,*,#4735,.F.);
#6224=ORIENTED_EDGE('',*,*,#4736,.T.);
#6225=ORIENTED_EDGE('',*,*,#4737,.F.);
#6226=ORIENTED_EDGE('',*,*,#4736,.F.);
#6227=ORIENTED_EDGE('',*,*,#4738,.F.);
#6228=ORIENTED_EDGE('',*,*,#4739,.T.);
#6229=ORIENTED_EDGE('',*,*,#4740,.F.);
#6230=ORIENTED_EDGE('',*,*,#4739,.F.);
#6231=ORIENTED_EDGE('',*,*,#4741,.F.);
#6232=ORIENTED_EDGE('',*,*,#4742,.T.);
#6233=ORIENTED_EDGE('',*,*,#4743,.F.);
#6234=ORIENTED_EDGE('',*,*,#4742,.F.);
#6235=ORIENTED_EDGE('',*,*,#4744,.F.);
#6236=ORIENTED_EDGE('',*,*,#4745,.T.);
#6237=ORIENTED_EDGE('',*,*,#4746,.F.);
#6238=ORIENTED_EDGE('',*,*,#4745,.F.);
#6239=ORIENTED_EDGE('',*,*,#4747,.F.);
#6240=ORIENTED_EDGE('',*,*,#4748,.T.);
#6241=ORIENTED_EDGE('',*,*,#4749,.F.);
#6242=ORIENTED_EDGE('',*,*,#4748,.F.);
#6243=ORIENTED_EDGE('',*,*,#4750,.F.);
#6244=ORIENTED_EDGE('',*,*,#4751,.T.);
#6245=ORIENTED_EDGE('',*,*,#4752,.F.);
#6246=ORIENTED_EDGE('',*,*,#4751,.F.);
#6247=ORIENTED_EDGE('',*,*,#4753,.F.);
#6248=ORIENTED_EDGE('',*,*,#4754,.T.);
#6249=ORIENTED_EDGE('',*,*,#4755,.F.);
#6250=ORIENTED_EDGE('',*,*,#4754,.F.);
#6251=ORIENTED_EDGE('',*,*,#4756,.F.);
#6252=ORIENTED_EDGE('',*,*,#4757,.T.);
#6253=ORIENTED_EDGE('',*,*,#4758,.F.);
#6254=ORIENTED_EDGE('',*,*,#4757,.F.);
#6255=ORIENTED_EDGE('',*,*,#4759,.F.);
#6256=ORIENTED_EDGE('',*,*,#4760,.T.);
#6257=ORIENTED_EDGE('',*,*,#4761,.F.);
#6258=ORIENTED_EDGE('',*,*,#4760,.F.);
#6259=ORIENTED_EDGE('',*,*,#4762,.F.);
#6260=ORIENTED_EDGE('',*,*,#4763,.T.);
#6261=ORIENTED_EDGE('',*,*,#4764,.F.);
#6262=ORIENTED_EDGE('',*,*,#4763,.F.);
#6263=ORIENTED_EDGE('',*,*,#4765,.F.);
#6264=ORIENTED_EDGE('',*,*,#4766,.T.);
#6265=ORIENTED_EDGE('',*,*,#4767,.F.);
#6266=ORIENTED_EDGE('',*,*,#4766,.F.);
#6267=ORIENTED_EDGE('',*,*,#4768,.F.);
#6268=ORIENTED_EDGE('',*,*,#4769,.T.);
#6269=ORIENTED_EDGE('',*,*,#4770,.F.);
#6270=ORIENTED_EDGE('',*,*,#4769,.F.);
#6271=ORIENTED_EDGE('',*,*,#4771,.F.);
#6272=ORIENTED_EDGE('',*,*,#4772,.T.);
#6273=ORIENTED_EDGE('',*,*,#4773,.F.);
#6274=ORIENTED_EDGE('',*,*,#4772,.F.);
#6275=ORIENTED_EDGE('',*,*,#4774,.F.);
#6276=ORIENTED_EDGE('',*,*,#4775,.T.);
#6277=ORIENTED_EDGE('',*,*,#4776,.F.);
#6278=ORIENTED_EDGE('',*,*,#4775,.F.);
#6279=ORIENTED_EDGE('',*,*,#4777,.F.);
#6280=ORIENTED_EDGE('',*,*,#4778,.T.);
#6281=ORIENTED_EDGE('',*,*,#4779,.F.);
#6282=ORIENTED_EDGE('',*,*,#4778,.F.);
#6283=ORIENTED_EDGE('',*,*,#4780,.F.);
#6284=ORIENTED_EDGE('',*,*,#4781,.T.);
#6285=ORIENTED_EDGE('',*,*,#4782,.F.);
#6286=ORIENTED_EDGE('',*,*,#4781,.F.);
#6287=ORIENTED_EDGE('',*,*,#4783,.F.);
#6288=ORIENTED_EDGE('',*,*,#4784,.T.);
#6289=ORIENTED_EDGE('',*,*,#4785,.F.);
#6290=ORIENTED_EDGE('',*,*,#4784,.F.);
#6291=ORIENTED_EDGE('',*,*,#4786,.F.);
#6292=ORIENTED_EDGE('',*,*,#4787,.T.);
#6293=ORIENTED_EDGE('',*,*,#4788,.F.);
#6294=ORIENTED_EDGE('',*,*,#4787,.F.);
#6295=ORIENTED_EDGE('',*,*,#4789,.T.);
#6296=ORIENTED_EDGE('',*,*,#4790,.T.);
#6297=ORIENTED_EDGE('',*,*,#4791,.F.);
#6298=ORIENTED_EDGE('',*,*,#4792,.F.);
#6299=ORIENTED_EDGE('',*,*,#4793,.T.);
#6300=ORIENTED_EDGE('',*,*,#4792,.T.);
#6301=ORIENTED_EDGE('',*,*,#4794,.F.);
#6302=ORIENTED_EDGE('',*,*,#4795,.F.);
#6303=ORIENTED_EDGE('',*,*,#4796,.T.);
#6304=ORIENTED_EDGE('',*,*,#4795,.T.);
#6305=ORIENTED_EDGE('',*,*,#4797,.F.);
#6306=ORIENTED_EDGE('',*,*,#4798,.F.);
#6307=ORIENTED_EDGE('',*,*,#4799,.T.);
#6308=ORIENTED_EDGE('',*,*,#4798,.T.);
#6309=ORIENTED_EDGE('',*,*,#4800,.F.);
#6310=ORIENTED_EDGE('',*,*,#4790,.F.);
#6311=ORIENTED_EDGE('',*,*,#4800,.T.);
#6312=ORIENTED_EDGE('',*,*,#4797,.T.);
#6313=ORIENTED_EDGE('',*,*,#4794,.T.);
#6314=ORIENTED_EDGE('',*,*,#4791,.T.);
#6315=ORIENTED_EDGE('',*,*,#4740,.T.);
#6316=ORIENTED_EDGE('',*,*,#4755,.T.);
#6317=ORIENTED_EDGE('',*,*,#4758,.T.);
#6318=ORIENTED_EDGE('',*,*,#4761,.T.);
#6319=ORIENTED_EDGE('',*,*,#4764,.T.);
#6320=ORIENTED_EDGE('',*,*,#4788,.T.);
#6321=ORIENTED_EDGE('',*,*,#4785,.T.);
#6322=ORIENTED_EDGE('',*,*,#4782,.T.);
#6323=ORIENTED_EDGE('',*,*,#4779,.T.);
#6324=ORIENTED_EDGE('',*,*,#4776,.T.);
#6325=ORIENTED_EDGE('',*,*,#4773,.T.);
#6326=ORIENTED_EDGE('',*,*,#4770,.T.);
#6327=ORIENTED_EDGE('',*,*,#4767,.T.);
#6328=ORIENTED_EDGE('',*,*,#4752,.T.);
#6329=ORIENTED_EDGE('',*,*,#4749,.T.);
#6330=ORIENTED_EDGE('',*,*,#4746,.T.);
#6331=ORIENTED_EDGE('',*,*,#4743,.T.);
#6332=ORIENTED_EDGE('',*,*,#4737,.T.);
#6333=ORIENTED_EDGE('',*,*,#4734,.T.);
#6334=ORIENTED_EDGE('',*,*,#4799,.F.);
#6335=ORIENTED_EDGE('',*,*,#4789,.F.);
#6336=ORIENTED_EDGE('',*,*,#4793,.F.);
#6337=ORIENTED_EDGE('',*,*,#4796,.F.);
#6338=ORIENTED_EDGE('',*,*,#4738,.T.);
#6339=ORIENTED_EDGE('',*,*,#4753,.T.);
#6340=ORIENTED_EDGE('',*,*,#4756,.T.);
#6341=ORIENTED_EDGE('',*,*,#4759,.T.);
#6342=ORIENTED_EDGE('',*,*,#4762,.T.);
#6343=ORIENTED_EDGE('',*,*,#4786,.T.);
#6344=ORIENTED_EDGE('',*,*,#4783,.T.);
#6345=ORIENTED_EDGE('',*,*,#4780,.T.);
#6346=ORIENTED_EDGE('',*,*,#4777,.T.);
#6347=ORIENTED_EDGE('',*,*,#4774,.T.);
#6348=ORIENTED_EDGE('',*,*,#4771,.T.);
#6349=ORIENTED_EDGE('',*,*,#4768,.T.);
#6350=ORIENTED_EDGE('',*,*,#4765,.T.);
#6351=ORIENTED_EDGE('',*,*,#4750,.T.);
#6352=ORIENTED_EDGE('',*,*,#4747,.T.);
#6353=ORIENTED_EDGE('',*,*,#4744,.T.);
#6354=ORIENTED_EDGE('',*,*,#4741,.T.);
#6355=ORIENTED_EDGE('',*,*,#4735,.T.);
#6356=ORIENTED_EDGE('',*,*,#4732,.T.);
#6357=ORIENTED_EDGE('',*,*,#4801,.F.);
#6358=ORIENTED_EDGE('',*,*,#4802,.T.);
#6359=ORIENTED_EDGE('',*,*,#4803,.T.);
#6360=ORIENTED_EDGE('',*,*,#4802,.F.);
#6361=ORIENTED_EDGE('',*,*,#4804,.F.);
#6362=ORIENTED_EDGE('',*,*,#4805,.T.);
#6363=ORIENTED_EDGE('',*,*,#4806,.T.);
#6364=ORIENTED_EDGE('',*,*,#4805,.F.);
#6365=ORIENTED_EDGE('',*,*,#4804,.T.);
#6366=ORIENTED_EDGE('',*,*,#4801,.T.);
#6367=ORIENTED_EDGE('',*,*,#4806,.F.);
#6368=ORIENTED_EDGE('',*,*,#4803,.F.);
#6369=ORIENTED_EDGE('',*,*,#4807,.F.);
#6370=ORIENTED_EDGE('',*,*,#4808,.T.);
#6371=ORIENTED_EDGE('',*,*,#4809,.F.);
#6372=ORIENTED_EDGE('',*,*,#4808,.F.);
#6373=ORIENTED_EDGE('',*,*,#4810,.F.);
#6374=ORIENTED_EDGE('',*,*,#4811,.T.);
#6375=ORIENTED_EDGE('',*,*,#4812,.F.);
#6376=ORIENTED_EDGE('',*,*,#4811,.F.);
#6377=ORIENTED_EDGE('',*,*,#4813,.T.);
#6378=ORIENTED_EDGE('',*,*,#4814,.T.);
#6379=ORIENTED_EDGE('',*,*,#4815,.F.);
#6380=ORIENTED_EDGE('',*,*,#4816,.F.);
#6381=ORIENTED_EDGE('',*,*,#4809,.T.);
#6382=ORIENTED_EDGE('',*,*,#4812,.T.);
#6383=ORIENTED_EDGE('',*,*,#4817,.T.);
#6384=ORIENTED_EDGE('',*,*,#4816,.T.);
#6385=ORIENTED_EDGE('',*,*,#4818,.F.);
#6386=ORIENTED_EDGE('',*,*,#4819,.F.);
#6387=ORIENTED_EDGE('',*,*,#4820,.T.);
#6388=ORIENTED_EDGE('',*,*,#4819,.T.);
#6389=ORIENTED_EDGE('',*,*,#4821,.F.);
#6390=ORIENTED_EDGE('',*,*,#4822,.F.);
#6391=ORIENTED_EDGE('',*,*,#4823,.T.);
#6392=ORIENTED_EDGE('',*,*,#4822,.T.);
#6393=ORIENTED_EDGE('',*,*,#4824,.F.);
#6394=ORIENTED_EDGE('',*,*,#4825,.F.);
#6395=ORIENTED_EDGE('',*,*,#4826,.T.);
#6396=ORIENTED_EDGE('',*,*,#4825,.T.);
#6397=ORIENTED_EDGE('',*,*,#4827,.F.);
#6398=ORIENTED_EDGE('',*,*,#4828,.F.);
#6399=ORIENTED_EDGE('',*,*,#4807,.T.);
#6400=ORIENTED_EDGE('',*,*,#4810,.T.);
#6401=ORIENTED_EDGE('',*,*,#4829,.T.);
#6402=ORIENTED_EDGE('',*,*,#4828,.T.);
#6403=ORIENTED_EDGE('',*,*,#4830,.F.);
#6404=ORIENTED_EDGE('',*,*,#4814,.F.);
#6405=ORIENTED_EDGE('',*,*,#4830,.T.);
#6406=ORIENTED_EDGE('',*,*,#4827,.T.);
#6407=ORIENTED_EDGE('',*,*,#4824,.T.);
#6408=ORIENTED_EDGE('',*,*,#4821,.T.);
#6409=ORIENTED_EDGE('',*,*,#4818,.T.);
#6410=ORIENTED_EDGE('',*,*,#4815,.T.);
#6411=ORIENTED_EDGE('',*,*,#4829,.F.);
#6412=ORIENTED_EDGE('',*,*,#4813,.F.);
#6413=ORIENTED_EDGE('',*,*,#4817,.F.);
#6414=ORIENTED_EDGE('',*,*,#4820,.F.);
#6415=ORIENTED_EDGE('',*,*,#4823,.F.);
#6416=ORIENTED_EDGE('',*,*,#4826,.F.);
#6417=ORIENTED_EDGE('',*,*,#4831,.F.);
#6418=ORIENTED_EDGE('',*,*,#4832,.T.);
#6419=ORIENTED_EDGE('',*,*,#4833,.F.);
#6420=ORIENTED_EDGE('',*,*,#4834,.F.);
#6421=ORIENTED_EDGE('',*,*,#4835,.T.);
#6422=ORIENTED_EDGE('',*,*,#4836,.F.);
#6423=ORIENTED_EDGE('',*,*,#4835,.F.);
#6424=ORIENTED_EDGE('',*,*,#4837,.F.);
#6425=ORIENTED_EDGE('',*,*,#4838,.F.);
#6426=ORIENTED_EDGE('',*,*,#4832,.F.);
#6427=ORIENTED_EDGE('',*,*,#4839,.F.);
#6428=ORIENTED_EDGE('',*,*,#4840,.T.);
#6429=ORIENTED_EDGE('',*,*,#4841,.F.);
#6430=ORIENTED_EDGE('',*,*,#4842,.F.);
#6431=ORIENTED_EDGE('',*,*,#4843,.T.);
#6432=ORIENTED_EDGE('',*,*,#4844,.F.);
#6433=ORIENTED_EDGE('',*,*,#4843,.F.);
#6434=ORIENTED_EDGE('',*,*,#4845,.F.);
#6435=ORIENTED_EDGE('',*,*,#4846,.F.);
#6436=ORIENTED_EDGE('',*,*,#4840,.F.);
#6437=ORIENTED_EDGE('',*,*,#4847,.F.);
#6438=ORIENTED_EDGE('',*,*,#4848,.T.);
#6439=ORIENTED_EDGE('',*,*,#4849,.F.);
#6440=ORIENTED_EDGE('',*,*,#4850,.F.);
#6441=ORIENTED_EDGE('',*,*,#4851,.T.);
#6442=ORIENTED_EDGE('',*,*,#4852,.F.);
#6443=ORIENTED_EDGE('',*,*,#4851,.F.);
#6444=ORIENTED_EDGE('',*,*,#4853,.F.);
#6445=ORIENTED_EDGE('',*,*,#4854,.F.);
#6446=ORIENTED_EDGE('',*,*,#4848,.F.);
#6447=ORIENTED_EDGE('',*,*,#4855,.F.);
#6448=ORIENTED_EDGE('',*,*,#4856,.T.);
#6449=ORIENTED_EDGE('',*,*,#4857,.F.);
#6450=ORIENTED_EDGE('',*,*,#4858,.F.);
#6451=ORIENTED_EDGE('',*,*,#4859,.T.);
#6452=ORIENTED_EDGE('',*,*,#4860,.F.);
#6453=ORIENTED_EDGE('',*,*,#4859,.F.);
#6454=ORIENTED_EDGE('',*,*,#4861,.F.);
#6455=ORIENTED_EDGE('',*,*,#4862,.F.);
#6456=ORIENTED_EDGE('',*,*,#4856,.F.);
#6457=ORIENTED_EDGE('',*,*,#4833,.T.);
#6458=ORIENTED_EDGE('',*,*,#4831,.T.);
#6459=ORIENTED_EDGE('',*,*,#4838,.T.);
#6460=ORIENTED_EDGE('',*,*,#4863,.T.);
#6461=ORIENTED_EDGE('',*,*,#4849,.T.);
#6462=ORIENTED_EDGE('',*,*,#4847,.T.);
#6463=ORIENTED_EDGE('',*,*,#4854,.T.);
#6464=ORIENTED_EDGE('',*,*,#4864,.T.);
#6465=ORIENTED_EDGE('',*,*,#4865,.F.);
#6466=ORIENTED_EDGE('',*,*,#4866,.T.);
#6467=ORIENTED_EDGE('',*,*,#4867,.F.);
#6468=ORIENTED_EDGE('',*,*,#4868,.T.);
#6469=ORIENTED_EDGE('',*,*,#4841,.T.);
#6470=ORIENTED_EDGE('',*,*,#4839,.T.);
#6471=ORIENTED_EDGE('',*,*,#4846,.T.);
#6472=ORIENTED_EDGE('',*,*,#4869,.T.);
#6473=ORIENTED_EDGE('',*,*,#4857,.T.);
#6474=ORIENTED_EDGE('',*,*,#4855,.T.);
#6475=ORIENTED_EDGE('',*,*,#4862,.T.);
#6476=ORIENTED_EDGE('',*,*,#4870,.T.);
#6477=ORIENTED_EDGE('',*,*,#4871,.F.);
#6478=ORIENTED_EDGE('',*,*,#4872,.F.);
#6479=ORIENTED_EDGE('',*,*,#4873,.F.);
#6480=ORIENTED_EDGE('',*,*,#4874,.T.);
#6481=ORIENTED_EDGE('',*,*,#4865,.T.);
#6482=ORIENTED_EDGE('',*,*,#4875,.T.);
#6483=ORIENTED_EDGE('',*,*,#4876,.T.);
#6484=ORIENTED_EDGE('',*,*,#4877,.T.);
#6485=ORIENTED_EDGE('',*,*,#4878,.T.);
#6486=ORIENTED_EDGE('',*,*,#4879,.T.);
#6487=ORIENTED_EDGE('',*,*,#4873,.T.);
#6488=ORIENTED_EDGE('',*,*,#4880,.T.);
#6489=ORIENTED_EDGE('',*,*,#4881,.T.);
#6490=ORIENTED_EDGE('',*,*,#4882,.T.);
#6491=ORIENTED_EDGE('',*,*,#4883,.T.);
#6492=ORIENTED_EDGE('',*,*,#4884,.T.);
#6493=ORIENTED_EDGE('',*,*,#4837,.T.);
#6494=ORIENTED_EDGE('',*,*,#4834,.T.);
#6495=ORIENTED_EDGE('',*,*,#4868,.F.);
#6496=ORIENTED_EDGE('',*,*,#4885,.F.);
#6497=ORIENTED_EDGE('',*,*,#4886,.F.);
#6498=ORIENTED_EDGE('',*,*,#4875,.F.);
#6499=ORIENTED_EDGE('',*,*,#4864,.F.);
#6500=ORIENTED_EDGE('',*,*,#4853,.T.);
#6501=ORIENTED_EDGE('',*,*,#4850,.T.);
#6502=ORIENTED_EDGE('',*,*,#4863,.F.);
#6503=ORIENTED_EDGE('',*,*,#4886,.T.);
#6504=ORIENTED_EDGE('',*,*,#4887,.F.);
#6505=ORIENTED_EDGE('',*,*,#4888,.F.);
#6506=ORIENTED_EDGE('',*,*,#4876,.F.);
#6507=ORIENTED_EDGE('',*,*,#4888,.T.);
#6508=ORIENTED_EDGE('',*,*,#4889,.F.);
#6509=ORIENTED_EDGE('',*,*,#4890,.F.);
#6510=ORIENTED_EDGE('',*,*,#4877,.F.);
#6511=ORIENTED_EDGE('',*,*,#4836,.T.);
#6512=ORIENTED_EDGE('',*,*,#4844,.T.);
#6513=ORIENTED_EDGE('',*,*,#4852,.T.);
#6514=ORIENTED_EDGE('',*,*,#4860,.T.);
#6515=ORIENTED_EDGE('',*,*,#4890,.T.);
#6516=ORIENTED_EDGE('',*,*,#4891,.F.);
#6517=ORIENTED_EDGE('',*,*,#4892,.F.);
#6518=ORIENTED_EDGE('',*,*,#4878,.F.);
#6519=ORIENTED_EDGE('',*,*,#4845,.T.);
#6520=ORIENTED_EDGE('',*,*,#4842,.T.);
#6521=ORIENTED_EDGE('',*,*,#4874,.F.);
#6522=ORIENTED_EDGE('',*,*,#4879,.F.);
#6523=ORIENTED_EDGE('',*,*,#4892,.T.);
#6524=ORIENTED_EDGE('',*,*,#4893,.F.);
#6525=ORIENTED_EDGE('',*,*,#4870,.F.);
#6526=ORIENTED_EDGE('',*,*,#4861,.T.);
#6527=ORIENTED_EDGE('',*,*,#4858,.T.);
#6528=ORIENTED_EDGE('',*,*,#4869,.F.);
#6529=ORIENTED_EDGE('',*,*,#4872,.T.);
#6530=ORIENTED_EDGE('',*,*,#4894,.F.);
#6531=ORIENTED_EDGE('',*,*,#4895,.F.);
#6532=ORIENTED_EDGE('',*,*,#4880,.F.);
#6533=ORIENTED_EDGE('',*,*,#4895,.T.);
#6534=ORIENTED_EDGE('',*,*,#4896,.F.);
#6535=ORIENTED_EDGE('',*,*,#4897,.F.);
#6536=ORIENTED_EDGE('',*,*,#4881,.F.);
#6537=ORIENTED_EDGE('',*,*,#4897,.T.);
#6538=ORIENTED_EDGE('',*,*,#4898,.F.);
#6539=ORIENTED_EDGE('',*,*,#4899,.F.);
#6540=ORIENTED_EDGE('',*,*,#4882,.F.);
#6541=ORIENTED_EDGE('',*,*,#4899,.T.);
#6542=ORIENTED_EDGE('',*,*,#4900,.F.);
#6543=ORIENTED_EDGE('',*,*,#4901,.F.);
#6544=ORIENTED_EDGE('',*,*,#4883,.F.);
#6545=ORIENTED_EDGE('',*,*,#4901,.T.);
#6546=ORIENTED_EDGE('',*,*,#4902,.F.);
#6547=ORIENTED_EDGE('',*,*,#4866,.F.);
#6548=ORIENTED_EDGE('',*,*,#4884,.F.);
#6549=ORIENTED_EDGE('',*,*,#4867,.T.);
#6550=ORIENTED_EDGE('',*,*,#4902,.T.);
#6551=ORIENTED_EDGE('',*,*,#4900,.T.);
#6552=ORIENTED_EDGE('',*,*,#4898,.T.);
#6553=ORIENTED_EDGE('',*,*,#4896,.T.);
#6554=ORIENTED_EDGE('',*,*,#4894,.T.);
#6555=ORIENTED_EDGE('',*,*,#4871,.T.);
#6556=ORIENTED_EDGE('',*,*,#4893,.T.);
#6557=ORIENTED_EDGE('',*,*,#4891,.T.);
#6558=ORIENTED_EDGE('',*,*,#4889,.T.);
#6559=ORIENTED_EDGE('',*,*,#4887,.T.);
#6560=ORIENTED_EDGE('',*,*,#4885,.T.);
#6561=ORIENTED_EDGE('',*,*,#4903,.T.);
#6562=ORIENTED_EDGE('',*,*,#4904,.T.);
#6563=ORIENTED_EDGE('',*,*,#4905,.F.);
#6564=ORIENTED_EDGE('',*,*,#4906,.F.);
#6565=ORIENTED_EDGE('',*,*,#4907,.T.);
#6566=ORIENTED_EDGE('',*,*,#4906,.T.);
#6567=ORIENTED_EDGE('',*,*,#4908,.F.);
#6568=ORIENTED_EDGE('',*,*,#4909,.F.);
#6569=ORIENTED_EDGE('',*,*,#4910,.T.);
#6570=ORIENTED_EDGE('',*,*,#4909,.T.);
#6571=ORIENTED_EDGE('',*,*,#4911,.F.);
#6572=ORIENTED_EDGE('',*,*,#4912,.F.);
#6573=ORIENTED_EDGE('',*,*,#4913,.T.);
#6574=ORIENTED_EDGE('',*,*,#4912,.T.);
#6575=ORIENTED_EDGE('',*,*,#4914,.F.);
#6576=ORIENTED_EDGE('',*,*,#4915,.F.);
#6577=ORIENTED_EDGE('',*,*,#4916,.T.);
#6578=ORIENTED_EDGE('',*,*,#4915,.T.);
#6579=ORIENTED_EDGE('',*,*,#4917,.F.);
#6580=ORIENTED_EDGE('',*,*,#4918,.F.);
#6581=ORIENTED_EDGE('',*,*,#4919,.T.);
#6582=ORIENTED_EDGE('',*,*,#4918,.T.);
#6583=ORIENTED_EDGE('',*,*,#4920,.F.);
#6584=ORIENTED_EDGE('',*,*,#4921,.F.);
#6585=ORIENTED_EDGE('',*,*,#4922,.T.);
#6586=ORIENTED_EDGE('',*,*,#4921,.T.);
#6587=ORIENTED_EDGE('',*,*,#4923,.F.);
#6588=ORIENTED_EDGE('',*,*,#4924,.F.);
#6589=ORIENTED_EDGE('',*,*,#4925,.T.);
#6590=ORIENTED_EDGE('',*,*,#4924,.T.);
#6591=ORIENTED_EDGE('',*,*,#4926,.F.);
#6592=ORIENTED_EDGE('',*,*,#4904,.F.);
#6593=ORIENTED_EDGE('',*,*,#4926,.T.);
#6594=ORIENTED_EDGE('',*,*,#4923,.T.);
#6595=ORIENTED_EDGE('',*,*,#4920,.T.);
#6596=ORIENTED_EDGE('',*,*,#4917,.T.);
#6597=ORIENTED_EDGE('',*,*,#4914,.T.);
#6598=ORIENTED_EDGE('',*,*,#4911,.T.);
#6599=ORIENTED_EDGE('',*,*,#4908,.T.);
#6600=ORIENTED_EDGE('',*,*,#4905,.T.);
#6601=ORIENTED_EDGE('',*,*,#4925,.F.);
#6602=ORIENTED_EDGE('',*,*,#4903,.F.);
#6603=ORIENTED_EDGE('',*,*,#4907,.F.);
#6604=ORIENTED_EDGE('',*,*,#4910,.F.);
#6605=ORIENTED_EDGE('',*,*,#4913,.F.);
#6606=ORIENTED_EDGE('',*,*,#4916,.F.);
#6607=ORIENTED_EDGE('',*,*,#4919,.F.);
#6608=ORIENTED_EDGE('',*,*,#4922,.F.);
#6609=ORIENTED_EDGE('',*,*,#4927,.F.);
#6610=ORIENTED_EDGE('',*,*,#4928,.T.);
#6611=ORIENTED_EDGE('',*,*,#4929,.F.);
#6612=ORIENTED_EDGE('',*,*,#4930,.F.);
#6613=ORIENTED_EDGE('',*,*,#4931,.F.);
#6614=ORIENTED_EDGE('',*,*,#4930,.T.);
#6615=ORIENTED_EDGE('',*,*,#4932,.F.);
#6616=ORIENTED_EDGE('',*,*,#4933,.F.);
#6617=ORIENTED_EDGE('',*,*,#4934,.F.);
#6618=ORIENTED_EDGE('',*,*,#4933,.T.);
#6619=ORIENTED_EDGE('',*,*,#4935,.F.);
#6620=ORIENTED_EDGE('',*,*,#4936,.F.);
#6621=ORIENTED_EDGE('',*,*,#4937,.F.);
#6622=ORIENTED_EDGE('',*,*,#4936,.T.);
#6623=ORIENTED_EDGE('',*,*,#4938,.F.);
#6624=ORIENTED_EDGE('',*,*,#4939,.F.);
#6625=ORIENTED_EDGE('',*,*,#4940,.F.);
#6626=ORIENTED_EDGE('',*,*,#4939,.T.);
#6627=ORIENTED_EDGE('',*,*,#4941,.F.);
#6628=ORIENTED_EDGE('',*,*,#4942,.F.);
#6629=ORIENTED_EDGE('',*,*,#4943,.F.);
#6630=ORIENTED_EDGE('',*,*,#4942,.T.);
#6631=ORIENTED_EDGE('',*,*,#4944,.F.);
#6632=ORIENTED_EDGE('',*,*,#4945,.F.);
#6633=ORIENTED_EDGE('',*,*,#4946,.F.);
#6634=ORIENTED_EDGE('',*,*,#4945,.T.);
#6635=ORIENTED_EDGE('',*,*,#4947,.F.);
#6636=ORIENTED_EDGE('',*,*,#4948,.F.);
#6637=ORIENTED_EDGE('',*,*,#4949,.F.);
#6638=ORIENTED_EDGE('',*,*,#4948,.T.);
#6639=ORIENTED_EDGE('',*,*,#4950,.F.);
#6640=ORIENTED_EDGE('',*,*,#4928,.F.);
#6641=ORIENTED_EDGE('',*,*,#4949,.T.);
#6642=ORIENTED_EDGE('',*,*,#4927,.T.);
#6643=ORIENTED_EDGE('',*,*,#4931,.T.);
#6644=ORIENTED_EDGE('',*,*,#4934,.T.);
#6645=ORIENTED_EDGE('',*,*,#4937,.T.);
#6646=ORIENTED_EDGE('',*,*,#4940,.T.);
#6647=ORIENTED_EDGE('',*,*,#4943,.T.);
#6648=ORIENTED_EDGE('',*,*,#4946,.T.);
#6649=ORIENTED_EDGE('',*,*,#4950,.T.);
#6650=ORIENTED_EDGE('',*,*,#4947,.T.);
#6651=ORIENTED_EDGE('',*,*,#4944,.T.);
#6652=ORIENTED_EDGE('',*,*,#4941,.T.);
#6653=ORIENTED_EDGE('',*,*,#4938,.T.);
#6654=ORIENTED_EDGE('',*,*,#4935,.T.);
#6655=ORIENTED_EDGE('',*,*,#4932,.T.);
#6656=ORIENTED_EDGE('',*,*,#4929,.T.);
#6657=ORIENTED_EDGE('',*,*,#4951,.T.);
#6658=ORIENTED_EDGE('',*,*,#4952,.T.);
#6659=ORIENTED_EDGE('',*,*,#4953,.T.);
#6660=ORIENTED_EDGE('',*,*,#4952,.F.);
#6661=ORIENTED_EDGE('',*,*,#4953,.F.);
#6662=ORIENTED_EDGE('',*,*,#4954,.T.);
#6663=ORIENTED_EDGE('',*,*,#4955,.T.);
#6664=ORIENTED_EDGE('',*,*,#4954,.F.);
#6665=ORIENTED_EDGE('',*,*,#4956,.T.);
#6666=ORIENTED_EDGE('',*,*,#4951,.F.);
#6667=ORIENTED_EDGE('',*,*,#4956,.F.);
#6668=ORIENTED_EDGE('',*,*,#4957,.T.);
#6669=ORIENTED_EDGE('',*,*,#4958,.T.);
#6670=ORIENTED_EDGE('',*,*,#4957,.F.);
#6671=ORIENTED_EDGE('',*,*,#4958,.F.);
#6672=ORIENTED_EDGE('',*,*,#4955,.F.);
#6673=ORIENTED_EDGE('',*,*,#4959,.F.);
#6674=ORIENTED_EDGE('',*,*,#4960,.F.);
#6675=ORIENTED_EDGE('',*,*,#4961,.T.);
#6676=ORIENTED_EDGE('',*,*,#4959,.T.);
#6677=ORIENTED_EDGE('',*,*,#4961,.F.);
#6678=ORIENTED_EDGE('',*,*,#4962,.F.);
#6679=ORIENTED_EDGE('',*,*,#4963,.T.);
#6680=ORIENTED_EDGE('',*,*,#4960,.T.);
#6681=ORIENTED_EDGE('',*,*,#4963,.F.);
#6682=ORIENTED_EDGE('',*,*,#4964,.F.);
#6683=ORIENTED_EDGE('',*,*,#4965,.T.);
#6684=ORIENTED_EDGE('',*,*,#4962,.T.);
#6685=ORIENTED_EDGE('',*,*,#4965,.F.);
#6686=ORIENTED_EDGE('',*,*,#4964,.T.);
#6687=ORIENTED_EDGE('',*,*,#4966,.F.);
#6688=ORIENTED_EDGE('',*,*,#4967,.F.);
#6689=ORIENTED_EDGE('',*,*,#4968,.T.);
#6690=ORIENTED_EDGE('',*,*,#4966,.T.);
#6691=ORIENTED_EDGE('',*,*,#4968,.F.);
#6692=ORIENTED_EDGE('',*,*,#4969,.F.);
#6693=ORIENTED_EDGE('',*,*,#4970,.T.);
#6694=ORIENTED_EDGE('',*,*,#4967,.T.);
#6695=ORIENTED_EDGE('',*,*,#4970,.F.);
#6696=ORIENTED_EDGE('',*,*,#4971,.F.);
#6697=ORIENTED_EDGE('',*,*,#4972,.T.);
#6698=ORIENTED_EDGE('',*,*,#4969,.T.);
#6699=ORIENTED_EDGE('',*,*,#4972,.F.);
#6700=ORIENTED_EDGE('',*,*,#4971,.T.);
#6701=ORIENTED_EDGE('',*,*,#4973,.T.);
#6702=ORIENTED_EDGE('',*,*,#4974,.T.);
#6703=ORIENTED_EDGE('',*,*,#4975,.T.);
#6704=ORIENTED_EDGE('',*,*,#4976,.F.);
#6705=ORIENTED_EDGE('',*,*,#4977,.T.);
#6706=ORIENTED_EDGE('',*,*,#4978,.T.);
#6707=ORIENTED_EDGE('',*,*,#4979,.T.);
#6708=ORIENTED_EDGE('',*,*,#4974,.F.);
#6709=ORIENTED_EDGE('',*,*,#4980,.T.);
#6710=ORIENTED_EDGE('',*,*,#4981,.T.);
#6711=ORIENTED_EDGE('',*,*,#4982,.T.);
#6712=ORIENTED_EDGE('',*,*,#4978,.F.);
#6713=ORIENTED_EDGE('',*,*,#4983,.T.);
#6714=ORIENTED_EDGE('',*,*,#4984,.T.);
#6715=ORIENTED_EDGE('',*,*,#4985,.T.);
#6716=ORIENTED_EDGE('',*,*,#4981,.F.);
#6717=ORIENTED_EDGE('',*,*,#4986,.T.);
#6718=ORIENTED_EDGE('',*,*,#4987,.T.);
#6719=ORIENTED_EDGE('',*,*,#4988,.T.);
#6720=ORIENTED_EDGE('',*,*,#4984,.F.);
#6721=ORIENTED_EDGE('',*,*,#4989,.T.);
#6722=ORIENTED_EDGE('',*,*,#4976,.T.);
#6723=ORIENTED_EDGE('',*,*,#4990,.T.);
#6724=ORIENTED_EDGE('',*,*,#4987,.F.);
#6725=ORIENTED_EDGE('',*,*,#4989,.F.);
#6726=ORIENTED_EDGE('',*,*,#4986,.F.);
#6727=ORIENTED_EDGE('',*,*,#4983,.F.);
#6728=ORIENTED_EDGE('',*,*,#4980,.F.);
#6729=ORIENTED_EDGE('',*,*,#4977,.F.);
#6730=ORIENTED_EDGE('',*,*,#4973,.F.);
#6731=ORIENTED_EDGE('',*,*,#4990,.F.);
#6732=ORIENTED_EDGE('',*,*,#4975,.F.);
#6733=ORIENTED_EDGE('',*,*,#4979,.F.);
#6734=ORIENTED_EDGE('',*,*,#4982,.F.);
#6735=ORIENTED_EDGE('',*,*,#4985,.F.);
#6736=ORIENTED_EDGE('',*,*,#4988,.F.);
#6737=ORIENTED_EDGE('',*,*,#4991,.F.);
#6738=ORIENTED_EDGE('',*,*,#4992,.T.);
#6739=ORIENTED_EDGE('',*,*,#4993,.T.);
#6740=ORIENTED_EDGE('',*,*,#4992,.F.);
#6741=ORIENTED_EDGE('',*,*,#4994,.F.);
#6742=ORIENTED_EDGE('',*,*,#4995,.T.);
#6743=ORIENTED_EDGE('',*,*,#4996,.T.);
#6744=ORIENTED_EDGE('',*,*,#4995,.F.);
#6745=ORIENTED_EDGE('',*,*,#4994,.T.);
#6746=ORIENTED_EDGE('',*,*,#4991,.T.);
#6747=ORIENTED_EDGE('',*,*,#4996,.F.);
#6748=ORIENTED_EDGE('',*,*,#4993,.F.);
#6749=ORIENTED_EDGE('',*,*,#4997,.F.);
#6750=ORIENTED_EDGE('',*,*,#4998,.F.);
#6751=ORIENTED_EDGE('',*,*,#4999,.T.);
#6752=ORIENTED_EDGE('',*,*,#4997,.T.);
#6753=ORIENTED_EDGE('',*,*,#4999,.F.);
#6754=ORIENTED_EDGE('',*,*,#5000,.F.);
#6755=ORIENTED_EDGE('',*,*,#5001,.T.);
#6756=ORIENTED_EDGE('',*,*,#4998,.T.);
#6757=ORIENTED_EDGE('',*,*,#5001,.F.);
#6758=ORIENTED_EDGE('',*,*,#5002,.F.);
#6759=ORIENTED_EDGE('',*,*,#5003,.T.);
#6760=ORIENTED_EDGE('',*,*,#5000,.T.);
#6761=ORIENTED_EDGE('',*,*,#5003,.F.);
#6762=ORIENTED_EDGE('',*,*,#5002,.T.);
#6763=ORIENTED_EDGE('',*,*,#5004,.F.);
#6764=ORIENTED_EDGE('',*,*,#5005,.F.);
#6765=ORIENTED_EDGE('',*,*,#5006,.T.);
#6766=ORIENTED_EDGE('',*,*,#5004,.T.);
#6767=ORIENTED_EDGE('',*,*,#5006,.F.);
#6768=ORIENTED_EDGE('',*,*,#5007,.F.);
#6769=ORIENTED_EDGE('',*,*,#5008,.T.);
#6770=ORIENTED_EDGE('',*,*,#5005,.T.);
#6771=ORIENTED_EDGE('',*,*,#5008,.F.);
#6772=ORIENTED_EDGE('',*,*,#5009,.F.);
#6773=ORIENTED_EDGE('',*,*,#5010,.T.);
#6774=ORIENTED_EDGE('',*,*,#5007,.T.);
#6775=ORIENTED_EDGE('',*,*,#5010,.F.);
#6776=ORIENTED_EDGE('',*,*,#5009,.T.);
#6777=ORIENTED_EDGE('',*,*,#5011,.T.);
#6778=ORIENTED_EDGE('',*,*,#5012,.T.);
#6779=ORIENTED_EDGE('',*,*,#5013,.T.);
#6780=ORIENTED_EDGE('',*,*,#5014,.F.);
#6781=ORIENTED_EDGE('',*,*,#5015,.T.);
#6782=ORIENTED_EDGE('',*,*,#5016,.T.);
#6783=ORIENTED_EDGE('',*,*,#5017,.T.);
#6784=ORIENTED_EDGE('',*,*,#5012,.F.);
#6785=ORIENTED_EDGE('',*,*,#5018,.T.);
#6786=ORIENTED_EDGE('',*,*,#5019,.T.);
#6787=ORIENTED_EDGE('',*,*,#5020,.T.);
#6788=ORIENTED_EDGE('',*,*,#5016,.F.);
#6789=ORIENTED_EDGE('',*,*,#5021,.T.);
#6790=ORIENTED_EDGE('',*,*,#5022,.T.);
#6791=ORIENTED_EDGE('',*,*,#5023,.T.);
#6792=ORIENTED_EDGE('',*,*,#5019,.F.);
#6793=ORIENTED_EDGE('',*,*,#5024,.T.);
#6794=ORIENTED_EDGE('',*,*,#5025,.T.);
#6795=ORIENTED_EDGE('',*,*,#5026,.T.);
#6796=ORIENTED_EDGE('',*,*,#5022,.F.);
#6797=ORIENTED_EDGE('',*,*,#5027,.T.);
#6798=ORIENTED_EDGE('',*,*,#5014,.T.);
#6799=ORIENTED_EDGE('',*,*,#5028,.T.);
#6800=ORIENTED_EDGE('',*,*,#5025,.F.);
#6801=ORIENTED_EDGE('',*,*,#5027,.F.);
#6802=ORIENTED_EDGE('',*,*,#5024,.F.);
#6803=ORIENTED_EDGE('',*,*,#5021,.F.);
#6804=ORIENTED_EDGE('',*,*,#5018,.F.);
#6805=ORIENTED_EDGE('',*,*,#5015,.F.);
#6806=ORIENTED_EDGE('',*,*,#5011,.F.);
#6807=ORIENTED_EDGE('',*,*,#5028,.F.);
#6808=ORIENTED_EDGE('',*,*,#5013,.F.);
#6809=ORIENTED_EDGE('',*,*,#5017,.F.);
#6810=ORIENTED_EDGE('',*,*,#5020,.F.);
#6811=ORIENTED_EDGE('',*,*,#5023,.F.);
#6812=ORIENTED_EDGE('',*,*,#5026,.F.);
#6813=ORIENTED_EDGE('',*,*,#5029,.T.);
#6814=ORIENTED_EDGE('',*,*,#5030,.T.);
#6815=ORIENTED_EDGE('',*,*,#5031,.T.);
#6816=ORIENTED_EDGE('',*,*,#5030,.F.);
#6817=ORIENTED_EDGE('',*,*,#5031,.F.);
#6818=ORIENTED_EDGE('',*,*,#5032,.T.);
#6819=ORIENTED_EDGE('',*,*,#5033,.T.);
#6820=ORIENTED_EDGE('',*,*,#5032,.F.);
#6821=ORIENTED_EDGE('',*,*,#5034,.T.);
#6822=ORIENTED_EDGE('',*,*,#5029,.F.);
#6823=ORIENTED_EDGE('',*,*,#5034,.F.);
#6824=ORIENTED_EDGE('',*,*,#5035,.T.);
#6825=ORIENTED_EDGE('',*,*,#5036,.T.);
#6826=ORIENTED_EDGE('',*,*,#5035,.F.);
#6827=ORIENTED_EDGE('',*,*,#5036,.F.);
#6828=ORIENTED_EDGE('',*,*,#5033,.F.);
#6829=ORIENTED_EDGE('',*,*,#5037,.T.);
#6830=ORIENTED_EDGE('',*,*,#5038,.T.);
#6831=ORIENTED_EDGE('',*,*,#5039,.T.);
#6832=ORIENTED_EDGE('',*,*,#5040,.F.);
#6833=ORIENTED_EDGE('',*,*,#5041,.T.);
#6834=ORIENTED_EDGE('',*,*,#5042,.T.);
#6835=ORIENTED_EDGE('',*,*,#5043,.T.);
#6836=ORIENTED_EDGE('',*,*,#5038,.F.);
#6837=ORIENTED_EDGE('',*,*,#5044,.T.);
#6838=ORIENTED_EDGE('',*,*,#5045,.T.);
#6839=ORIENTED_EDGE('',*,*,#5046,.T.);
#6840=ORIENTED_EDGE('',*,*,#5042,.F.);
#6841=ORIENTED_EDGE('',*,*,#5047,.T.);
#6842=ORIENTED_EDGE('',*,*,#5048,.T.);
#6843=ORIENTED_EDGE('',*,*,#5049,.T.);
#6844=ORIENTED_EDGE('',*,*,#5045,.F.);
#6845=ORIENTED_EDGE('',*,*,#5050,.T.);
#6846=ORIENTED_EDGE('',*,*,#5051,.T.);
#6847=ORIENTED_EDGE('',*,*,#5052,.T.);
#6848=ORIENTED_EDGE('',*,*,#5048,.F.);
#6849=ORIENTED_EDGE('',*,*,#5053,.T.);
#6850=ORIENTED_EDGE('',*,*,#5040,.T.);
#6851=ORIENTED_EDGE('',*,*,#5054,.T.);
#6852=ORIENTED_EDGE('',*,*,#5051,.F.);
#6853=ORIENTED_EDGE('',*,*,#5053,.F.);
#6854=ORIENTED_EDGE('',*,*,#5050,.F.);
#6855=ORIENTED_EDGE('',*,*,#5047,.F.);
#6856=ORIENTED_EDGE('',*,*,#5044,.F.);
#6857=ORIENTED_EDGE('',*,*,#5041,.F.);
#6858=ORIENTED_EDGE('',*,*,#5037,.F.);
#6859=ORIENTED_EDGE('',*,*,#5054,.F.);
#6860=ORIENTED_EDGE('',*,*,#5039,.F.);
#6861=ORIENTED_EDGE('',*,*,#5043,.F.);
#6862=ORIENTED_EDGE('',*,*,#5046,.F.);
#6863=ORIENTED_EDGE('',*,*,#5049,.F.);
#6864=ORIENTED_EDGE('',*,*,#5052,.F.);
#6865=ORIENTED_EDGE('',*,*,#5055,.F.);
#6866=ORIENTED_EDGE('',*,*,#5056,.F.);
#6867=ORIENTED_EDGE('',*,*,#5057,.F.);
#6868=ORIENTED_EDGE('',*,*,#5058,.T.);
#6869=ORIENTED_EDGE('',*,*,#5056,.T.);
#6870=ORIENTED_EDGE('',*,*,#5058,.F.);
#6871=ORIENTED_EDGE('',*,*,#5059,.F.);
#6872=ORIENTED_EDGE('',*,*,#5060,.T.);
#6873=ORIENTED_EDGE('',*,*,#5057,.T.);
#6874=ORIENTED_EDGE('',*,*,#5060,.F.);
#6875=ORIENTED_EDGE('',*,*,#5061,.F.);
#6876=ORIENTED_EDGE('',*,*,#5062,.T.);
#6877=ORIENTED_EDGE('',*,*,#5059,.T.);
#6878=ORIENTED_EDGE('',*,*,#5062,.F.);
#6879=ORIENTED_EDGE('',*,*,#5061,.T.);
#6880=ORIENTED_EDGE('',*,*,#5063,.F.);
#6881=ORIENTED_EDGE('',*,*,#5064,.F.);
#6882=ORIENTED_EDGE('',*,*,#5065,.T.);
#6883=ORIENTED_EDGE('',*,*,#5063,.T.);
#6884=ORIENTED_EDGE('',*,*,#5065,.F.);
#6885=ORIENTED_EDGE('',*,*,#5055,.T.);
#6886=ORIENTED_EDGE('',*,*,#5066,.T.);
#6887=ORIENTED_EDGE('',*,*,#5064,.T.);
#6888=ORIENTED_EDGE('',*,*,#5066,.F.);
#6889=CYLINDRICAL_SURFACE('',#7744,0.164999999999999);
#6890=CYLINDRICAL_SURFACE('',#7747,0.164999999999999);
#6891=CYLINDRICAL_SURFACE('',#7750,0.164999999999999);
#6892=CYLINDRICAL_SURFACE('',#7753,0.164999999999999);
#6893=CYLINDRICAL_SURFACE('',#7756,0.275);
#6894=CYLINDRICAL_SURFACE('',#7759,0.274999999999999);
#6895=CYLINDRICAL_SURFACE('',#7769,0.164999999999999);
#6896=CYLINDRICAL_SURFACE('',#7772,0.164999999999999);
#6897=CYLINDRICAL_SURFACE('',#7775,0.164999999999999);
#6898=CYLINDRICAL_SURFACE('',#7778,0.164999999999999);
#6899=CYLINDRICAL_SURFACE('',#7781,0.275);
#6900=CYLINDRICAL_SURFACE('',#7784,0.274999999999999);
#6901=CYLINDRICAL_SURFACE('',#7794,0.275);
#6902=CYLINDRICAL_SURFACE('',#7797,0.275);
#6903=CYLINDRICAL_SURFACE('',#7807,0.275);
#6904=CYLINDRICAL_SURFACE('',#7810,0.275);
#6905=CYLINDRICAL_SURFACE('',#7834,0.274999999999999);
#6906=CYLINDRICAL_SURFACE('',#7837,0.274999999999999);
#6907=CYLINDRICAL_SURFACE('',#7847,0.274999999999999);
#6908=CYLINDRICAL_SURFACE('',#7850,0.274999999999999);
#6909=CYLINDRICAL_SURFACE('',#7874,0.5);
#6910=CYLINDRICAL_SURFACE('',#7877,0.5);
#6911=CYLINDRICAL_SURFACE('',#7882,0.5);
#6912=CYLINDRICAL_SURFACE('',#7885,0.5);
#6913=CYLINDRICAL_SURFACE('',#7893,0.275);
#6914=CYLINDRICAL_SURFACE('',#7895,0.275);
#6915=CYLINDRICAL_SURFACE('',#7910,0.5);
#6916=CYLINDRICAL_SURFACE('',#7913,0.5);
#6917=CYLINDRICAL_SURFACE('',#7918,0.5);
#6918=CYLINDRICAL_SURFACE('',#7921,0.5);
#6919=CYLINDRICAL_SURFACE('',#7929,0.274999999999999);
#6920=CYLINDRICAL_SURFACE('',#7931,0.274999999999999);
#6921=CYLINDRICAL_SURFACE('',#7982,0.21);
#6922=CYLINDRICAL_SURFACE('',#7996,0.375);
#6923=CYLINDRICAL_SURFACE('',#8001,0.375);
#6924=CYLINDRICAL_SURFACE('',#8006,0.375);
#6925=CYLINDRICAL_SURFACE('',#8011,0.375);
#6926=CYLINDRICAL_SURFACE('',#8016,0.225);
#6927=CYLINDRICAL_SURFACE('',#8018,0.225);
#6928=CYLINDRICAL_SURFACE('',#8020,0.225);
#6929=CYLINDRICAL_SURFACE('',#8022,0.225000000000001);
#6930=CYLINDRICAL_SURFACE('',#8043,0.35);
#6931=CYLINDRICAL_SURFACE('',#8051,0.1954);
#6932=CYLINDRICAL_SURFACE('',#8076,0.2117);
#6933=CYLINDRICAL_SURFACE('',#8100,0.425);
#6934=CYLINDRICAL_SURFACE('',#8108,0.24505);
#6935=CYLINDRICAL_SURFACE('',#8111,0.164999999999999);
#6936=CYLINDRICAL_SURFACE('',#8114,0.164999999999999);
#6937=CYLINDRICAL_SURFACE('',#8117,0.25);
#6938=CYLINDRICAL_SURFACE('',#8120,0.274999999999999);
#6939=CYLINDRICAL_SURFACE('',#8123,0.274999999999999);
#6940=CYLINDRICAL_SURFACE('',#8126,0.274999999999999);
#6941=CYLINDRICAL_SURFACE('',#8129,0.274999999999999);
#6942=CYLINDRICAL_SURFACE('',#8132,0.274999999999999);
#6943=CYLINDRICAL_SURFACE('',#8135,0.275);
#6944=CYLINDRICAL_SURFACE('',#8138,0.275);
#6945=CYLINDRICAL_SURFACE('',#8141,0.274999999999999);
#6946=CYLINDRICAL_SURFACE('',#8144,0.274999999999999);
#6947=CYLINDRICAL_SURFACE('',#8147,0.274999999999999);
#6948=CYLINDRICAL_SURFACE('',#8150,0.274999999999999);
#6949=CYLINDRICAL_SURFACE('',#8153,0.274999999999999);
#6950=CYLINDRICAL_SURFACE('',#8156,0.274999999999999);
#6951=CYLINDRICAL_SURFACE('',#8159,0.275);
#6952=CYLINDRICAL_SURFACE('',#8162,0.275);
#6953=CYLINDRICAL_SURFACE('',#8165,0.274999999999999);
#6954=CYLINDRICAL_SURFACE('',#8175,0.329999999999998);
#6955=CYLINDRICAL_SURFACE('',#8178,1.5);
#6956=CYLINDRICAL_SURFACE('',#8184,0.225000000000001);
#6957=CYLINDRICAL_SURFACE('',#8187,0.225000000000001);
#6958=CYLINDRICAL_SURFACE('',#8202,0.21);
#6959=CYLINDRICAL_SURFACE('',#8208,0.21);
#6960=CYLINDRICAL_SURFACE('',#8214,0.21);
#6961=CYLINDRICAL_SURFACE('',#8220,0.21);
#6962=CYLINDRICAL_SURFACE('',#8267,0.265);
#6963=CYLINDRICAL_SURFACE('',#8271,0.5);
#6964=CYLINDRICAL_SURFACE('',#8349,0.425);
#6965=CYLINDRICAL_SURFACE('',#8357,0.24505);
#6966=CYLINDRICAL_SURFACE('',#8371,0.32);
#6967=CYLINDRICAL_SURFACE('',#8374,0.6);
#6968=CYLINDRICAL_SURFACE('',#8384,0.5);
#6969=CYLINDRICAL_SURFACE('',#8392,0.2942);
#6970=CYLINDRICAL_SURFACE('',#8409,0.215);
#6971=CYLINDRICAL_SURFACE('',#8413,0.45);
#6972=CYLINDRICAL_SURFACE('',#8431,0.35);
#6973=CYLINDRICAL_SURFACE('',#8439,0.1954);
#6974=ADVANCED_FACE('',(#1048),#6889,.F.);
#6975=ADVANCED_FACE('',(#1049),#6890,.F.);
#6976=ADVANCED_FACE('',(#1050),#6891,.F.);
#6977=ADVANCED_FACE('',(#1051),#6892,.F.);
#6978=ADVANCED_FACE('',(#1052),#6893,.F.);
#6979=ADVANCED_FACE('',(#1053),#6894,.F.);
#6980=ADVANCED_FACE('',(#1054),#764,.T.);
#6981=ADVANCED_FACE('',(#1055),#765,.T.);
#6982=ADVANCED_FACE('',(#1056),#766,.T.);
#6983=ADVANCED_FACE('',(#1057),#767,.T.);
#6984=ADVANCED_FACE('',(#1058,#642,#643,#644,#645,#646,#647),#768,.T.);
#6985=ADVANCED_FACE('',(#1059,#648,#649,#650,#651,#652,#653),#769,.F.);
#6986=ADVANCED_FACE('',(#1060),#6895,.F.);
#6987=ADVANCED_FACE('',(#1061),#6896,.F.);
#6988=ADVANCED_FACE('',(#1062),#6897,.F.);
#6989=ADVANCED_FACE('',(#1063),#6898,.F.);
#6990=ADVANCED_FACE('',(#1064),#6899,.F.);
#6991=ADVANCED_FACE('',(#1065),#6900,.F.);
#6992=ADVANCED_FACE('',(#1066),#770,.T.);
#6993=ADVANCED_FACE('',(#1067),#771,.T.);
#6994=ADVANCED_FACE('',(#1068),#772,.T.);
#6995=ADVANCED_FACE('',(#1069),#773,.T.);
#6996=ADVANCED_FACE('',(#1070,#654,#655,#656,#657,#658,#659),#774,.T.);
#6997=ADVANCED_FACE('',(#1071,#660,#661,#662,#663,#664,#665),#775,.F.);
#6998=ADVANCED_FACE('',(#1072),#6901,.F.);
#6999=ADVANCED_FACE('',(#1073),#6902,.F.);
#7000=ADVANCED_FACE('',(#1074),#776,.T.);
#7001=ADVANCED_FACE('',(#1075),#777,.T.);
#7002=ADVANCED_FACE('',(#1076),#778,.T.);
#7003=ADVANCED_FACE('',(#1077),#779,.T.);
#7004=ADVANCED_FACE('',(#1078,#666,#667),#780,.T.);
#7005=ADVANCED_FACE('',(#1079,#668,#669),#781,.F.);
#7006=ADVANCED_FACE('',(#1080),#6903,.F.);
#7007=ADVANCED_FACE('',(#1081),#6904,.F.);
#7008=ADVANCED_FACE('',(#1082),#782,.T.);
#7009=ADVANCED_FACE('',(#1083),#783,.T.);
#7010=ADVANCED_FACE('',(#1084),#784,.T.);
#7011=ADVANCED_FACE('',(#1085),#785,.T.);
#7012=ADVANCED_FACE('',(#1086,#670,#671),#786,.T.);
#7013=ADVANCED_FACE('',(#1087,#672,#673),#787,.F.);
#7014=ADVANCED_FACE('',(#1088),#788,.T.);
#7015=ADVANCED_FACE('',(#1089),#789,.T.);
#7016=ADVANCED_FACE('',(#1090),#790,.T.);
#7017=ADVANCED_FACE('',(#1091),#791,.T.);
#7018=ADVANCED_FACE('',(#1092),#792,.T.);
#7019=ADVANCED_FACE('',(#1093),#793,.F.);
#7020=ADVANCED_FACE('',(#1094),#794,.T.);
#7021=ADVANCED_FACE('',(#1095),#795,.T.);
#7022=ADVANCED_FACE('',(#1096),#796,.T.);
#7023=ADVANCED_FACE('',(#1097),#797,.T.);
#7024=ADVANCED_FACE('',(#1098),#798,.T.);
#7025=ADVANCED_FACE('',(#1099),#799,.F.);
#7026=ADVANCED_FACE('',(#1100),#6905,.F.);
#7027=ADVANCED_FACE('',(#1101),#6906,.F.);
#7028=ADVANCED_FACE('',(#1102),#800,.T.);
#7029=ADVANCED_FACE('',(#1103),#801,.T.);
#7030=ADVANCED_FACE('',(#1104),#802,.T.);
#7031=ADVANCED_FACE('',(#1105),#803,.T.);
#7032=ADVANCED_FACE('',(#1106,#674,#675),#804,.T.);
#7033=ADVANCED_FACE('',(#1107,#676,#677),#805,.F.);
#7034=ADVANCED_FACE('',(#1108),#6907,.F.);
#7035=ADVANCED_FACE('',(#1109),#6908,.F.);
#7036=ADVANCED_FACE('',(#1110),#806,.T.);
#7037=ADVANCED_FACE('',(#1111),#807,.T.);
#7038=ADVANCED_FACE('',(#1112),#808,.T.);
#7039=ADVANCED_FACE('',(#1113),#809,.T.);
#7040=ADVANCED_FACE('',(#1114,#678,#679),#810,.T.);
#7041=ADVANCED_FACE('',(#1115,#680,#681),#811,.F.);
#7042=ADVANCED_FACE('',(#1116),#812,.T.);
#7043=ADVANCED_FACE('',(#1117),#813,.T.);
#7044=ADVANCED_FACE('',(#1118),#814,.T.);
#7045=ADVANCED_FACE('',(#1119),#815,.T.);
#7046=ADVANCED_FACE('',(#1120),#816,.T.);
#7047=ADVANCED_FACE('',(#1121),#817,.F.);
#7048=ADVANCED_FACE('',(#1122),#818,.T.);
#7049=ADVANCED_FACE('',(#1123),#819,.T.);
#7050=ADVANCED_FACE('',(#1124),#820,.T.);
#7051=ADVANCED_FACE('',(#1125),#821,.T.);
#7052=ADVANCED_FACE('',(#1126),#822,.T.);
#7053=ADVANCED_FACE('',(#1127),#823,.F.);
#7054=ADVANCED_FACE('',(#1128),#6909,.F.);
#7055=ADVANCED_FACE('',(#1129),#6910,.F.);
#7056=ADVANCED_FACE('',(#1130,#682),#824,.T.);
#7057=ADVANCED_FACE('',(#1131),#6911,.F.);
#7058=ADVANCED_FACE('',(#1132),#6912,.F.);
#7059=ADVANCED_FACE('',(#1133,#683),#825,.T.);
#7060=ADVANCED_FACE('',(#1134),#826,.T.);
#7061=ADVANCED_FACE('',(#1135),#827,.T.);
#7062=ADVANCED_FACE('',(#1136),#828,.T.);
#7063=ADVANCED_FACE('',(#1137),#6913,.F.);
#7064=ADVANCED_FACE('',(#1138),#6914,.F.);
#7065=ADVANCED_FACE('',(#1139),#829,.T.);
#7066=ADVANCED_FACE('',(#1140),#830,.T.);
#7067=ADVANCED_FACE('',(#1141),#831,.T.);
#7068=ADVANCED_FACE('',(#1142),#832,.T.);
#7069=ADVANCED_FACE('',(#1143,#684,#685),#833,.F.);
#7070=ADVANCED_FACE('',(#1144),#834,.T.);
#7071=ADVANCED_FACE('',(#1145),#835,.T.);
#7072=ADVANCED_FACE('',(#1146),#836,.T.);
#7073=ADVANCED_FACE('',(#1147),#837,.T.);
#7074=ADVANCED_FACE('',(#1148),#838,.T.);
#7075=ADVANCED_FACE('',(#1149),#839,.F.);
#7076=ADVANCED_FACE('',(#1150),#6915,.F.);
#7077=ADVANCED_FACE('',(#1151),#6916,.F.);
#7078=ADVANCED_FACE('',(#1152,#686),#840,.T.);
#7079=ADVANCED_FACE('',(#1153),#6917,.F.);
#7080=ADVANCED_FACE('',(#1154),#6918,.F.);
#7081=ADVANCED_FACE('',(#1155,#687),#841,.T.);
#7082=ADVANCED_FACE('',(#1156),#842,.T.);
#7083=ADVANCED_FACE('',(#1157),#843,.T.);
#7084=ADVANCED_FACE('',(#1158),#844,.T.);
#7085=ADVANCED_FACE('',(#1159),#6919,.F.);
#7086=ADVANCED_FACE('',(#1160),#6920,.F.);
#7087=ADVANCED_FACE('',(#1161),#845,.T.);
#7088=ADVANCED_FACE('',(#1162),#846,.T.);
#7089=ADVANCED_FACE('',(#1163),#847,.T.);
#7090=ADVANCED_FACE('',(#1164),#848,.T.);
#7091=ADVANCED_FACE('',(#1165,#688,#689),#849,.F.);
#7092=ADVANCED_FACE('',(#1166),#850,.T.);
#7093=ADVANCED_FACE('',(#1167),#851,.T.);
#7094=ADVANCED_FACE('',(#1168),#852,.T.);
#7095=ADVANCED_FACE('',(#1169),#853,.T.);
#7096=ADVANCED_FACE('',(#1170),#854,.T.);
#7097=ADVANCED_FACE('',(#1171),#855,.F.);
#7098=ADVANCED_FACE('',(#1172),#856,.F.);
#7099=ADVANCED_FACE('',(#1173),#857,.F.);
#7100=ADVANCED_FACE('',(#1174),#858,.F.);
#7101=ADVANCED_FACE('',(#1175),#859,.F.);
#7102=ADVANCED_FACE('',(#1176),#860,.F.);
#7103=ADVANCED_FACE('',(#1177),#861,.F.);
#7104=ADVANCED_FACE('',(#1178),#862,.F.);
#7105=ADVANCED_FACE('',(#1179),#863,.F.);
#7106=ADVANCED_FACE('',(#1180),#864,.F.);
#7107=ADVANCED_FACE('',(#1181),#865,.F.);
#7108=ADVANCED_FACE('',(#1182),#866,.F.);
#7109=ADVANCED_FACE('',(#1183),#867,.F.);
#7110=ADVANCED_FACE('',(#1184),#868,.F.);
#7111=ADVANCED_FACE('',(#1185),#869,.F.);
#7112=ADVANCED_FACE('',(#1186),#870,.F.);
#7113=ADVANCED_FACE('',(#1187),#871,.F.);
#7114=ADVANCED_FACE('',(#1188),#872,.F.);
#7115=ADVANCED_FACE('',(#1189),#873,.F.);
#7116=ADVANCED_FACE('',(#1190),#874,.F.);
#7117=ADVANCED_FACE('',(#1191),#875,.F.);
#7118=ADVANCED_FACE('',(#1192),#876,.F.);
#7119=ADVANCED_FACE('',(#1193),#877,.F.);
#7120=ADVANCED_FACE('',(#1194),#878,.F.);
#7121=ADVANCED_FACE('',(#1195),#879,.F.);
#7122=ADVANCED_FACE('',(#1196),#880,.F.);
#7123=ADVANCED_FACE('',(#1197),#881,.F.);
#7124=ADVANCED_FACE('',(#1198),#882,.F.);
#7125=ADVANCED_FACE('',(#1199),#883,.F.);
#7126=ADVANCED_FACE('',(#1200),#884,.F.);
#7127=ADVANCED_FACE('',(#1201),#885,.F.);
#7128=ADVANCED_FACE('',(#1202),#886,.F.);
#7129=ADVANCED_FACE('',(#1203),#887,.F.);
#7130=ADVANCED_FACE('',(#1204),#888,.F.);
#7131=ADVANCED_FACE('',(#1205),#889,.F.);
#7132=ADVANCED_FACE('',(#1206),#890,.F.);
#7133=ADVANCED_FACE('',(#1207),#891,.F.);
#7134=ADVANCED_FACE('',(#1208),#6921,.F.);
#7135=ADVANCED_FACE('',(#1209),#892,.T.);
#7136=ADVANCED_FACE('',(#1210),#893,.T.);
#7137=ADVANCED_FACE('',(#1211),#894,.T.);
#7138=ADVANCED_FACE('',(#1212),#895,.T.);
#7139=ADVANCED_FACE('',(#1213),#896,.T.);
#7140=ADVANCED_FACE('',(#1214),#897,.T.);
#7141=ADVANCED_FACE('',(#1215),#898,.T.);
#7142=ADVANCED_FACE('',(#1216),#899,.T.);
#7143=ADVANCED_FACE('',(#1217,#690),#900,.T.);
#7144=ADVANCED_FACE('',(#1218,#691),#901,.F.);
#7145=ADVANCED_FACE('',(#1219),#6922,.F.);
#7146=ADVANCED_FACE('',(#1220,#692),#902,.T.);
#7147=ADVANCED_FACE('',(#1221),#6923,.F.);
#7148=ADVANCED_FACE('',(#1222,#693),#903,.T.);
#7149=ADVANCED_FACE('',(#1223),#6924,.F.);
#7150=ADVANCED_FACE('',(#1224,#694),#904,.T.);
#7151=ADVANCED_FACE('',(#1225),#6925,.F.);
#7152=ADVANCED_FACE('',(#1226,#695),#905,.T.);
#7153=ADVANCED_FACE('',(#1227),#6926,.F.);
#7154=ADVANCED_FACE('',(#1228),#6927,.F.);
#7155=ADVANCED_FACE('',(#1229),#6928,.F.);
#7156=ADVANCED_FACE('',(#1230),#6929,.F.);
#7157=ADVANCED_FACE('',(#1231),#906,.T.);
#7158=ADVANCED_FACE('',(#1232),#907,.T.);
#7159=ADVANCED_FACE('',(#1233),#908,.T.);
#7160=ADVANCED_FACE('',(#1234),#909,.T.);
#7161=ADVANCED_FACE('',(#1235,#696,#697,#698,#699),#910,.T.);
#7162=ADVANCED_FACE('',(#1236),#911,.T.);
#7163=ADVANCED_FACE('',(#1237),#912,.T.);
#7164=ADVANCED_FACE('',(#1238),#913,.T.);
#7165=ADVANCED_FACE('',(#1239),#914,.T.);
#7166=ADVANCED_FACE('',(#1240),#915,.T.);
#7167=ADVANCED_FACE('',(#1241,#700,#701,#702,#703),#916,.T.);
#7168=ADVANCED_FACE('',(#1242),#917,.T.);
#7169=ADVANCED_FACE('',(#1243),#918,.T.);
#7170=ADVANCED_FACE('',(#1244),#919,.F.);
#7171=ADVANCED_FACE('',(#1245),#920,.T.);
#7172=ADVANCED_FACE('',(#1246),#498,.T.);
#7173=ADVANCED_FACE('',(#1247),#6930,.T.);
#7174=ADVANCED_FACE('',(#1248),#499,.T.);
#7175=ADVANCED_FACE('',(#1249,#704),#921,.T.);
#7176=ADVANCED_FACE('',(#1250),#500,.T.);
#7177=ADVANCED_FACE('',(#1251),#6931,.T.);
#7178=ADVANCED_FACE('',(#1252),#501,.T.);
#7179=ADVANCED_FACE('',(#1253),#922,.T.);
#7180=ADVANCED_FACE('',(#1254),#923,.F.);
#7181=ADVANCED_FACE('',(#1255),#924,.F.);
#7182=ADVANCED_FACE('',(#1256),#925,.F.);
#7183=ADVANCED_FACE('',(#1257),#926,.F.);
#7184=ADVANCED_FACE('',(#1258),#927,.F.);
#7185=ADVANCED_FACE('',(#1259),#928,.F.);
#7186=ADVANCED_FACE('',(#1260),#929,.F.);
#7187=ADVANCED_FACE('',(#1261),#930,.F.);
#7188=ADVANCED_FACE('',(#1262),#931,.F.);
#7189=ADVANCED_FACE('',(#1263),#932,.T.);
#7190=ADVANCED_FACE('',(#1264,#705),#933,.T.);
#7191=ADVANCED_FACE('',(#1265),#934,.T.);
#7192=ADVANCED_FACE('',(#1266),#935,.T.);
#7193=ADVANCED_FACE('',(#1267),#936,.F.);
#7194=ADVANCED_FACE('',(#1268),#937,.T.);
#7195=ADVANCED_FACE('',(#1269),#938,.T.);
#7196=ADVANCED_FACE('',(#1270),#939,.T.);
#7197=ADVANCED_FACE('',(#1271),#6932,.F.);
#7198=ADVANCED_FACE('',(#1272),#940,.F.);
#7199=ADVANCED_FACE('',(#1273),#941,.F.);
#7200=ADVANCED_FACE('',(#1274),#942,.T.);
#7201=ADVANCED_FACE('',(#1275),#943,.T.);
#7202=ADVANCED_FACE('',(#1276),#944,.F.);
#7203=ADVANCED_FACE('',(#1277),#945,.F.);
#7204=ADVANCED_FACE('',(#1278),#946,.F.);
#7205=ADVANCED_FACE('',(#1279),#947,.F.);
#7206=ADVANCED_FACE('',(#1280),#948,.F.);
#7207=ADVANCED_FACE('',(#1281),#949,.F.);
#7208=ADVANCED_FACE('',(#1282),#950,.F.);
#7209=ADVANCED_FACE('',(#1283),#951,.F.);
#7210=ADVANCED_FACE('',(#1284),#952,.F.);
#7211=ADVANCED_FACE('',(#1285),#953,.T.);
#7212=ADVANCED_FACE('',(#1286),#502,.T.);
#7213=ADVANCED_FACE('',(#1287),#6933,.T.);
#7214=ADVANCED_FACE('',(#1288),#503,.T.);
#7215=ADVANCED_FACE('',(#1289,#706),#954,.T.);
#7216=ADVANCED_FACE('',(#1290),#504,.T.);
#7217=ADVANCED_FACE('',(#1291),#6934,.T.);
#7218=ADVANCED_FACE('',(#1292),#6935,.F.);
#7219=ADVANCED_FACE('',(#1293),#6936,.F.);
#7220=ADVANCED_FACE('',(#1294),#6937,.F.);
#7221=ADVANCED_FACE('',(#1295),#6938,.F.);
#7222=ADVANCED_FACE('',(#1296),#6939,.F.);
#7223=ADVANCED_FACE('',(#1297),#6940,.F.);
#7224=ADVANCED_FACE('',(#1298),#6941,.F.);
#7225=ADVANCED_FACE('',(#1299),#6942,.F.);
#7226=ADVANCED_FACE('',(#1300),#6943,.F.);
#7227=ADVANCED_FACE('',(#1301),#6944,.F.);
#7228=ADVANCED_FACE('',(#1302),#6945,.F.);
#7229=ADVANCED_FACE('',(#1303),#6946,.F.);
#7230=ADVANCED_FACE('',(#1304),#6947,.F.);
#7231=ADVANCED_FACE('',(#1305),#6948,.F.);
#7232=ADVANCED_FACE('',(#1306),#6949,.F.);
#7233=ADVANCED_FACE('',(#1307),#6950,.F.);
#7234=ADVANCED_FACE('',(#1308),#6951,.F.);
#7235=ADVANCED_FACE('',(#1309),#6952,.F.);
#7236=ADVANCED_FACE('',(#1310),#6953,.F.);
#7237=ADVANCED_FACE('',(#1311),#955,.T.);
#7238=ADVANCED_FACE('',(#1312),#956,.T.);
#7239=ADVANCED_FACE('',(#1313),#957,.T.);
#7240=ADVANCED_FACE('',(#1314),#958,.T.);
#7241=ADVANCED_FACE('',(#1315,#707,#708,#709,#710,#711,#712,#713,#714,#715,
#716,#717,#718,#719,#720,#721,#722,#723,#724,#725),#959,.T.);
#7242=ADVANCED_FACE('',(#1316,#726,#727,#728,#729,#730,#731,#732,#733,#734,
#735,#736,#737,#738,#739,#740,#741,#742,#743,#744),#960,.F.);
#7243=ADVANCED_FACE('',(#1317),#6954,.F.);
#7244=ADVANCED_FACE('',(#1318),#6955,.T.);
#7245=ADVANCED_FACE('',(#1319,#745),#961,.T.);
#7246=ADVANCED_FACE('',(#1320,#746),#962,.F.);
#7247=ADVANCED_FACE('',(#1321),#6956,.F.);
#7248=ADVANCED_FACE('',(#1322),#6957,.F.);
#7249=ADVANCED_FACE('',(#1323,#747,#748),#963,.T.);
#7250=ADVANCED_FACE('',(#1324),#964,.T.);
#7251=ADVANCED_FACE('',(#1325),#965,.T.);
#7252=ADVANCED_FACE('',(#1326),#966,.T.);
#7253=ADVANCED_FACE('',(#1327,#749,#750),#967,.T.);
#7254=ADVANCED_FACE('',(#1328),#968,.T.);
#7255=ADVANCED_FACE('',(#1329),#969,.T.);
#7256=ADVANCED_FACE('',(#1330),#970,.F.);
#7257=ADVANCED_FACE('',(#1331),#971,.T.);
#7258=ADVANCED_FACE('',(#1332),#6958,.F.);
#7259=ADVANCED_FACE('',(#1333),#972,.T.);
#7260=ADVANCED_FACE('',(#1334),#6959,.F.);
#7261=ADVANCED_FACE('',(#1335),#973,.T.);
#7262=ADVANCED_FACE('',(#1336),#6960,.F.);
#7263=ADVANCED_FACE('',(#1337),#974,.T.);
#7264=ADVANCED_FACE('',(#1338),#6961,.F.);
#7265=ADVANCED_FACE('',(#1339),#975,.T.);
#7266=ADVANCED_FACE('',(#1340),#976,.T.);
#7267=ADVANCED_FACE('',(#1341),#977,.T.);
#7268=ADVANCED_FACE('',(#1342),#978,.T.);
#7269=ADVANCED_FACE('',(#1343),#979,.T.);
#7270=ADVANCED_FACE('',(#1344,#751,#752,#753,#754),#980,.T.);
#7271=ADVANCED_FACE('',(#1345),#981,.T.);
#7272=ADVANCED_FACE('',(#1346),#982,.T.);
#7273=ADVANCED_FACE('',(#1347),#983,.T.);
#7274=ADVANCED_FACE('',(#1348),#984,.T.);
#7275=ADVANCED_FACE('',(#1349),#985,.T.);
#7276=ADVANCED_FACE('',(#1350),#986,.T.);
#7277=ADVANCED_FACE('',(#1351),#987,.T.);
#7278=ADVANCED_FACE('',(#1352),#988,.T.);
#7279=ADVANCED_FACE('',(#1353),#989,.T.);
#7280=ADVANCED_FACE('',(#1354),#990,.T.);
#7281=ADVANCED_FACE('',(#1355),#991,.T.);
#7282=ADVANCED_FACE('',(#1356),#992,.T.);
#7283=ADVANCED_FACE('',(#1357),#993,.T.);
#7284=ADVANCED_FACE('',(#1358),#994,.T.);
#7285=ADVANCED_FACE('',(#1359),#995,.T.);
#7286=ADVANCED_FACE('',(#1360),#996,.T.);
#7287=ADVANCED_FACE('',(#1361),#997,.T.);
#7288=ADVANCED_FACE('',(#1362),#998,.F.);
#7289=ADVANCED_FACE('',(#1363),#999,.T.);
#7290=ADVANCED_FACE('',(#1364),#1000,.T.);
#7291=ADVANCED_FACE('',(#1365),#1001,.T.);
#7292=ADVANCED_FACE('',(#1366),#1002,.T.);
#7293=ADVANCED_FACE('',(#1367),#1003,.T.);
#7294=ADVANCED_FACE('',(#1368),#1004,.T.);
#7295=ADVANCED_FACE('',(#1369),#1005,.T.);
#7296=ADVANCED_FACE('',(#1370),#1006,.T.);
#7297=ADVANCED_FACE('',(#1371),#1007,.T.);
#7298=ADVANCED_FACE('',(#1372),#1008,.T.);
#7299=ADVANCED_FACE('',(#1373),#505,.F.);
#7300=ADVANCED_FACE('',(#1374),#6962,.F.);
#7301=ADVANCED_FACE('',(#1375,#755),#1009,.T.);
#7302=ADVANCED_FACE('',(#1376),#6963,.T.);
#7303=ADVANCED_FACE('',(#1377,#756),#1010,.F.);
#7304=ADVANCED_FACE('',(#1378),#1011,.T.);
#7305=ADVANCED_FACE('',(#1379),#506,.T.);
#7306=ADVANCED_FACE('',(#1380),#6964,.T.);
#7307=ADVANCED_FACE('',(#1381),#507,.T.);
#7308=ADVANCED_FACE('',(#1382,#757),#1012,.T.);
#7309=ADVANCED_FACE('',(#1383),#508,.T.);
#7310=ADVANCED_FACE('',(#1384),#6965,.T.);
#7311=ADVANCED_FACE('',(#1385),#509,.T.);
#7312=ADVANCED_FACE('',(#1386),#1013,.T.);
#7313=ADVANCED_FACE('',(#1387),#1014,.F.);
#7314=ADVANCED_FACE('',(#1388),#1015,.F.);
#7315=ADVANCED_FACE('',(#1389),#1016,.F.);
#7316=ADVANCED_FACE('',(#1390),#1017,.F.);
#7317=ADVANCED_FACE('',(#1391),#1018,.F.);
#7318=ADVANCED_FACE('',(#1392),#1019,.F.);
#7319=ADVANCED_FACE('',(#1393),#1020,.F.);
#7320=ADVANCED_FACE('',(#1394),#1021,.F.);
#7321=ADVANCED_FACE('',(#1395),#6966,.F.);
#7322=ADVANCED_FACE('',(#1396),#6967,.T.);
#7323=ADVANCED_FACE('',(#1397,#758),#1022,.T.);
#7324=ADVANCED_FACE('',(#1398,#759),#1023,.F.);
#7325=ADVANCED_FACE('',(#1399),#1024,.T.);
#7326=ADVANCED_FACE('',(#1400),#510,.T.);
#7327=ADVANCED_FACE('',(#1401),#6968,.T.);
#7328=ADVANCED_FACE('',(#1402),#511,.T.);
#7329=ADVANCED_FACE('',(#1403,#760),#1025,.T.);
#7330=ADVANCED_FACE('',(#1404),#512,.T.);
#7331=ADVANCED_FACE('',(#1405),#6969,.T.);
#7332=ADVANCED_FACE('',(#1406),#513,.T.);
#7333=ADVANCED_FACE('',(#1407),#1026,.T.);
#7334=ADVANCED_FACE('',(#1408),#1027,.F.);
#7335=ADVANCED_FACE('',(#1409),#1028,.F.);
#7336=ADVANCED_FACE('',(#1410),#1029,.F.);
#7337=ADVANCED_FACE('',(#1411),#1030,.F.);
#7338=ADVANCED_FACE('',(#1412),#1031,.F.);
#7339=ADVANCED_FACE('',(#1413),#1032,.F.);
#7340=ADVANCED_FACE('',(#1414),#1033,.F.);
#7341=ADVANCED_FACE('',(#1415),#1034,.F.);
#7342=ADVANCED_FACE('',(#1416),#514,.F.);
#7343=ADVANCED_FACE('',(#1417),#6970,.F.);
#7344=ADVANCED_FACE('',(#1418,#761),#1035,.T.);
#7345=ADVANCED_FACE('',(#1419),#6971,.T.);
#7346=ADVANCED_FACE('',(#1420,#762),#1036,.F.);
#7347=ADVANCED_FACE('',(#1421),#1037,.F.);
#7348=ADVANCED_FACE('',(#1422),#1038,.F.);
#7349=ADVANCED_FACE('',(#1423),#1039,.F.);
#7350=ADVANCED_FACE('',(#1424),#1040,.F.);
#7351=ADVANCED_FACE('',(#1425),#1041,.F.);
#7352=ADVANCED_FACE('',(#1426),#1042,.F.);
#7353=ADVANCED_FACE('',(#1427),#1043,.F.);
#7354=ADVANCED_FACE('',(#1428),#1044,.F.);
#7355=ADVANCED_FACE('',(#1429),#1045,.F.);
#7356=ADVANCED_FACE('',(#1430),#1046,.T.);
#7357=ADVANCED_FACE('',(#1431),#515,.T.);
#7358=ADVANCED_FACE('',(#1432),#6972,.T.);
#7359=ADVANCED_FACE('',(#1433),#516,.T.);
#7360=ADVANCED_FACE('',(#1434,#763),#1047,.T.);
#7361=ADVANCED_FACE('',(#1435),#517,.T.);
#7362=ADVANCED_FACE('',(#1436),#6973,.T.);
#7363=CLOSED_SHELL('',(#6974,#6975,#6976,#6977,#6978,#6979,#6980,#6981,
#6982,#6983,#6984,#6985));
#7364=CLOSED_SHELL('',(#6986,#6987,#6988,#6989,#6990,#6991,#6992,#6993,
#6994,#6995,#6996,#6997));
#7365=CLOSED_SHELL('',(#6998,#6999,#7000,#7001,#7002,#7003,#7004,#7005));
#7366=CLOSED_SHELL('',(#7006,#7007,#7008,#7009,#7010,#7011,#7012,#7013));
#7367=CLOSED_SHELL('',(#7014,#7015,#7016,#7017,#7018,#7019));
#7368=CLOSED_SHELL('',(#7020,#7021,#7022,#7023,#7024,#7025));
#7369=CLOSED_SHELL('',(#7026,#7027,#7028,#7029,#7030,#7031,#7032,#7033));
#7370=CLOSED_SHELL('',(#7034,#7035,#7036,#7037,#7038,#7039,#7040,#7041));
#7371=CLOSED_SHELL('',(#7042,#7043,#7044,#7045,#7046,#7047));
#7372=CLOSED_SHELL('',(#7048,#7049,#7050,#7051,#7052,#7053));
#7373=CLOSED_SHELL('',(#7054,#7055,#7056,#7057,#7058,#7059,#7060,#7061,
#7062,#7063,#7064,#7065,#7066,#7067,#7068,#7069));
#7374=CLOSED_SHELL('',(#7070,#7071,#7072,#7073,#7074,#7075));
#7375=CLOSED_SHELL('',(#7076,#7077,#7078,#7079,#7080,#7081,#7082,#7083,
#7084,#7085,#7086,#7087,#7088,#7089,#7090,#7091));
#7376=CLOSED_SHELL('',(#7092,#7093,#7094,#7095,#7096,#7097));
#7377=CLOSED_SHELL('',(#7098,#7099,#7100,#7101,#7102,#7103,#7104,#7105,
#7106,#7107,#7108,#7109,#7110,#7111,#7112,#7113,#7114,#7115,#7116,#7117,
#7118,#7119,#7120,#7121,#7122,#7123,#7124,#7125,#7126,#7127,#7128,#7129,
#7130,#7131,#7132,#7133,#7134,#7135,#7136,#7137,#7138,#7139,#7140,#7141,
#7142,#7143,#7144));
#7378=CLOSED_SHELL('',(#7145,#7146,#7147,#7148,#7149,#7150,#7151,#7152,
#7153,#7154,#7155,#7156,#7157,#7158,#7159,#7160,#7161,#7162,#7163,#7164,
#7165,#7166,#7167,#7168,#7169,#7170));
#7379=CLOSED_SHELL('',(#7171,#7172,#7173,#7174,#7175,#7176,#7177,#7178,
#7179));
#7380=CLOSED_SHELL('',(#7180,#7181,#7182,#7183,#7184,#7185,#7186,#7187));
#7381=CLOSED_SHELL('',(#7188,#7189,#7190,#7191,#7192,#7193,#7194,#7195,
#7196,#7197,#7198,#7199,#7200,#7201));
#7382=CLOSED_SHELL('',(#7202,#7203,#7204,#7205,#7206,#7207,#7208,#7209));
#7383=CLOSED_SHELL('',(#7210,#7211,#7212,#7213,#7214,#7215,#7216,#7217));
#7384=CLOSED_SHELL('',(#7218,#7219,#7220,#7221,#7222,#7223,#7224,#7225,
#7226,#7227,#7228,#7229,#7230,#7231,#7232,#7233,#7234,#7235,#7236,#7237,
#7238,#7239,#7240,#7241,#7242));
#7385=CLOSED_SHELL('',(#7243,#7244,#7245,#7246));
#7386=CLOSED_SHELL('',(#7247,#7248,#7249,#7250,#7251,#7252,#7253,#7254,
#7255,#7256));
#7387=CLOSED_SHELL('',(#7257,#7258,#7259,#7260,#7261,#7262,#7263,#7264,
#7265,#7266,#7267,#7268,#7269,#7270,#7271,#7272,#7273,#7274,#7275,#7276,
#7277,#7278));
#7388=CLOSED_SHELL('',(#7279,#7280,#7281,#7282,#7283,#7284,#7285,#7286,
#7287,#7288));
#7389=CLOSED_SHELL('',(#7289,#7290,#7291,#7292,#7293,#7294,#7295,#7296,
#7297,#7298));
#7390=CLOSED_SHELL('',(#7299,#7300,#7301,#7302,#7303));
#7391=CLOSED_SHELL('',(#7304,#7305,#7306,#7307,#7308,#7309,#7310,#7311,
#7312));
#7392=CLOSED_SHELL('',(#7313,#7314,#7315,#7316,#7317,#7318,#7319,#7320));
#7393=CLOSED_SHELL('',(#7321,#7322,#7323,#7324));
#7394=CLOSED_SHELL('',(#7325,#7326,#7327,#7328,#7329,#7330,#7331,#7332,
#7333));
#7395=CLOSED_SHELL('',(#7334,#7335,#7336,#7337,#7338,#7339,#7340,#7341));
#7396=CLOSED_SHELL('',(#7342,#7343,#7344,#7345,#7346));
#7397=CLOSED_SHELL('',(#7347,#7348,#7349,#7350,#7351,#7352,#7353,#7354));
#7398=CLOSED_SHELL('',(#7355,#7356,#7357,#7358,#7359,#7360,#7361,#7362));
#7399=DERIVED_UNIT_ELEMENT(#7461,1.);
#7400=DERIVED_UNIT_ELEMENT(#12806,-3.);
#7401=DERIVED_UNIT_ELEMENT(#7461,1.);
#7402=DERIVED_UNIT_ELEMENT(#12806,-3.);
#7403=DERIVED_UNIT_ELEMENT(#7461,1.);
#7404=DERIVED_UNIT_ELEMENT(#12806,-3.);
#7405=DERIVED_UNIT_ELEMENT(#7461,1.);
#7406=DERIVED_UNIT_ELEMENT(#12806,-3.);
#7407=DERIVED_UNIT_ELEMENT(#7461,1.);
#7408=DERIVED_UNIT_ELEMENT(#12806,-3.);
#7409=DERIVED_UNIT_ELEMENT(#7461,1.);
#7410=DERIVED_UNIT_ELEMENT(#12806,-3.);
#7411=DERIVED_UNIT_ELEMENT(#7461,1.);
#7412=DERIVED_UNIT_ELEMENT(#12806,-3.);
#7413=DERIVED_UNIT_ELEMENT(#7461,1.);
#7414=DERIVED_UNIT_ELEMENT(#12806,-3.);
#7415=DERIVED_UNIT_ELEMENT(#7461,1.);
#7416=DERIVED_UNIT_ELEMENT(#12806,-3.);
#7417=DERIVED_UNIT_ELEMENT(#7461,1.);
#7418=DERIVED_UNIT_ELEMENT(#12806,-3.);
#7419=DERIVED_UNIT_ELEMENT(#7461,1.);
#7420=DERIVED_UNIT_ELEMENT(#12806,-3.);
#7421=DERIVED_UNIT_ELEMENT(#7461,1.);
#7422=DERIVED_UNIT_ELEMENT(#12806,-3.);
#7423=DERIVED_UNIT_ELEMENT(#7461,1.);
#7424=DERIVED_UNIT_ELEMENT(#12806,-3.);
#7425=DERIVED_UNIT_ELEMENT(#7461,1.);
#7426=DERIVED_UNIT_ELEMENT(#12806,-3.);
#7427=DERIVED_UNIT_ELEMENT(#7461,1.);
#7428=DERIVED_UNIT_ELEMENT(#12806,-3.);
#7429=DERIVED_UNIT_ELEMENT(#7461,1.);
#7430=DERIVED_UNIT_ELEMENT(#12806,-3.);
#7431=DERIVED_UNIT_ELEMENT(#7461,1.);
#7432=DERIVED_UNIT_ELEMENT(#12806,-3.);
#7433=DERIVED_UNIT_ELEMENT(#7461,1.);
#7434=DERIVED_UNIT_ELEMENT(#12806,-3.);
#7435=DERIVED_UNIT_ELEMENT(#7461,1.);
#7436=DERIVED_UNIT_ELEMENT(#12806,-3.);
#7437=DERIVED_UNIT_ELEMENT(#7461,1.);
#7438=DERIVED_UNIT_ELEMENT(#12806,-3.);
#7439=DERIVED_UNIT_ELEMENT(#7461,1.);
#7440=DERIVED_UNIT_ELEMENT(#12806,-3.);
#7441=DERIVED_UNIT_ELEMENT(#7461,1.);
#7442=DERIVED_UNIT_ELEMENT(#12806,-3.);
#7443=DERIVED_UNIT_ELEMENT(#7461,1.);
#7444=DERIVED_UNIT_ELEMENT(#12806,-3.);
#7445=DERIVED_UNIT_ELEMENT(#7461,1.);
#7446=DERIVED_UNIT_ELEMENT(#12806,-3.);
#7447=DERIVED_UNIT_ELEMENT(#7461,1.);
#7448=DERIVED_UNIT_ELEMENT(#12806,-3.);
#7449=DERIVED_UNIT_ELEMENT(#7461,1.);
#7450=DERIVED_UNIT_ELEMENT(#12806,-3.);
#7451=DERIVED_UNIT_ELEMENT(#7461,1.);
#7452=DERIVED_UNIT_ELEMENT(#12806,-3.);
#7453=DERIVED_UNIT_ELEMENT(#7461,1.);
#7454=DERIVED_UNIT_ELEMENT(#12806,-3.);
#7455=DERIVED_UNIT_ELEMENT(#7461,1.);
#7456=DERIVED_UNIT_ELEMENT(#12806,-3.);
#7457=DERIVED_UNIT_ELEMENT(#7461,1.);
#7458=DERIVED_UNIT_ELEMENT(#12806,-3.);
#7459=DERIVED_UNIT_ELEMENT(#7461,1.);
#7460=DERIVED_UNIT_ELEMENT(#12806,-3.);
#7461=(
MASS_UNIT()
NAMED_UNIT(*)
SI_UNIT(.KILO.,.GRAM.)
);
#7462=DERIVED_UNIT((#7399,#7400));
#7463=DERIVED_UNIT((#7401,#7402));
#7464=DERIVED_UNIT((#7403,#7404));
#7465=DERIVED_UNIT((#7405,#7406));
#7466=DERIVED_UNIT((#7407,#7408));
#7467=DERIVED_UNIT((#7409,#7410));
#7468=DERIVED_UNIT((#7411,#7412));
#7469=DERIVED_UNIT((#7413,#7414));
#7470=DERIVED_UNIT((#7415,#7416));
#7471=DERIVED_UNIT((#7417,#7418));
#7472=DERIVED_UNIT((#7419,#7420));
#7473=DERIVED_UNIT((#7421,#7422));
#7474=DERIVED_UNIT((#7423,#7424));
#7475=DERIVED_UNIT((#7425,#7426));
#7476=DERIVED_UNIT((#7427,#7428));
#7477=DERIVED_UNIT((#7429,#7430));
#7478=DERIVED_UNIT((#7431,#7432));
#7479=DERIVED_UNIT((#7433,#7434));
#7480=DERIVED_UNIT((#7435,#7436));
#7481=DERIVED_UNIT((#7437,#7438));
#7482=DERIVED_UNIT((#7439,#7440));
#7483=DERIVED_UNIT((#7441,#7442));
#7484=DERIVED_UNIT((#7443,#7444));
#7485=DERIVED_UNIT((#7445,#7446));
#7486=DERIVED_UNIT((#7447,#7448));
#7487=DERIVED_UNIT((#7449,#7450));
#7488=DERIVED_UNIT((#7451,#7452));
#7489=DERIVED_UNIT((#7453,#7454));
#7490=DERIVED_UNIT((#7455,#7456));
#7491=DERIVED_UNIT((#7457,#7458));
#7492=DERIVED_UNIT((#7459,#7460));
#7493=MEASURE_REPRESENTATION_ITEM('density measure',
POSITIVE_RATIO_MEASURE(7850.),#7462);
#7494=MEASURE_REPRESENTATION_ITEM('density measure',
POSITIVE_RATIO_MEASURE(7850.),#7463);
#7495=MEASURE_REPRESENTATION_ITEM('density measure',
POSITIVE_RATIO_MEASURE(7850.),#7464);
#7496=MEASURE_REPRESENTATION_ITEM('density measure',
POSITIVE_RATIO_MEASURE(7850.),#7465);
#7497=MEASURE_REPRESENTATION_ITEM('density measure',
POSITIVE_RATIO_MEASURE(7850.),#7466);
#7498=MEASURE_REPRESENTATION_ITEM('density measure',
POSITIVE_RATIO_MEASURE(7850.),#7467);
#7499=MEASURE_REPRESENTATION_ITEM('density measure',
POSITIVE_RATIO_MEASURE(7850.),#7468);
#7500=MEASURE_REPRESENTATION_ITEM('density measure',
POSITIVE_RATIO_MEASURE(7850.),#7469);
#7501=MEASURE_REPRESENTATION_ITEM('density measure',
POSITIVE_RATIO_MEASURE(7850.),#7470);
#7502=MEASURE_REPRESENTATION_ITEM('density measure',
POSITIVE_RATIO_MEASURE(7850.),#7471);
#7503=MEASURE_REPRESENTATION_ITEM('density measure',
POSITIVE_RATIO_MEASURE(7850.),#7472);
#7504=MEASURE_REPRESENTATION_ITEM('density measure',
POSITIVE_RATIO_MEASURE(7850.),#7473);
#7505=MEASURE_REPRESENTATION_ITEM('density measure',
POSITIVE_RATIO_MEASURE(7850.),#7474);
#7506=MEASURE_REPRESENTATION_ITEM('density measure',
POSITIVE_RATIO_MEASURE(7850.),#7475);
#7507=MEASURE_REPRESENTATION_ITEM('density measure',
POSITIVE_RATIO_MEASURE(7850.),#7476);
#7508=MEASURE_REPRESENTATION_ITEM('density measure',
POSITIVE_RATIO_MEASURE(7850.),#7477);
#7509=MEASURE_REPRESENTATION_ITEM('density measure',
POSITIVE_RATIO_MEASURE(7850.),#7478);
#7510=MEASURE_REPRESENTATION_ITEM('density measure',
POSITIVE_RATIO_MEASURE(7850.),#7479);
#7511=MEASURE_REPRESENTATION_ITEM('density measure',
POSITIVE_RATIO_MEASURE(7850.),#7480);
#7512=MEASURE_REPRESENTATION_ITEM('density measure',
POSITIVE_RATIO_MEASURE(7850.),#7481);
#7513=MEASURE_REPRESENTATION_ITEM('density measure',
POSITIVE_RATIO_MEASURE(7850.),#7482);
#7514=MEASURE_REPRESENTATION_ITEM('density measure',
POSITIVE_RATIO_MEASURE(7850.),#7483);
#7515=MEASURE_REPRESENTATION_ITEM('density measure',
POSITIVE_RATIO_MEASURE(7850.),#7484);
#7516=MEASURE_REPRESENTATION_ITEM('density measure',
POSITIVE_RATIO_MEASURE(7850.),#7485);
#7517=MEASURE_REPRESENTATION_ITEM('density measure',
POSITIVE_RATIO_MEASURE(7850.),#7486);
#7518=MEASURE_REPRESENTATION_ITEM('density measure',
POSITIVE_RATIO_MEASURE(7850.),#7487);
#7519=MEASURE_REPRESENTATION_ITEM('density measure',
POSITIVE_RATIO_MEASURE(7850.),#7488);
#7520=MEASURE_REPRESENTATION_ITEM('density measure',
POSITIVE_RATIO_MEASURE(7850.),#7489);
#7521=MEASURE_REPRESENTATION_ITEM('density measure',
POSITIVE_RATIO_MEASURE(7850.),#7490);
#7522=MEASURE_REPRESENTATION_ITEM('density measure',
POSITIVE_RATIO_MEASURE(7850.),#7491);
#7523=MEASURE_REPRESENTATION_ITEM('density measure',
POSITIVE_RATIO_MEASURE(7850.),#7492);
#7524=PROPERTY_DEFINITION_REPRESENTATION(#7679,#7586);
#7525=PROPERTY_DEFINITION_REPRESENTATION(#7680,#7587);
#7526=PROPERTY_DEFINITION_REPRESENTATION(#7681,#7588);
#7527=PROPERTY_DEFINITION_REPRESENTATION(#7682,#7589);
#7528=PROPERTY_DEFINITION_REPRESENTATION(#7683,#7590);
#7529=PROPERTY_DEFINITION_REPRESENTATION(#7684,#7591);
#7530=PROPERTY_DEFINITION_REPRESENTATION(#7685,#7592);
#7531=PROPERTY_DEFINITION_REPRESENTATION(#7686,#7593);
#7532=PROPERTY_DEFINITION_REPRESENTATION(#7687,#7594);
#7533=PROPERTY_DEFINITION_REPRESENTATION(#7688,#7595);
#7534=PROPERTY_DEFINITION_REPRESENTATION(#7689,#7596);
#7535=PROPERTY_DEFINITION_REPRESENTATION(#7690,#7597);
#7536=PROPERTY_DEFINITION_REPRESENTATION(#7691,#7598);
#7537=PROPERTY_DEFINITION_REPRESENTATION(#7692,#7599);
#7538=PROPERTY_DEFINITION_REPRESENTATION(#7693,#7600);
#7539=PROPERTY_DEFINITION_REPRESENTATION(#7694,#7601);
#7540=PROPERTY_DEFINITION_REPRESENTATION(#7695,#7602);
#7541=PROPERTY_DEFINITION_REPRESENTATION(#7696,#7603);
#7542=PROPERTY_DEFINITION_REPRESENTATION(#7697,#7604);
#7543=PROPERTY_DEFINITION_REPRESENTATION(#7698,#7605);
#7544=PROPERTY_DEFINITION_REPRESENTATION(#7699,#7606);
#7545=PROPERTY_DEFINITION_REPRESENTATION(#7700,#7607);
#7546=PROPERTY_DEFINITION_REPRESENTATION(#7701,#7608);
#7547=PROPERTY_DEFINITION_REPRESENTATION(#7702,#7609);
#7548=PROPERTY_DEFINITION_REPRESENTATION(#7703,#7610);
#7549=PROPERTY_DEFINITION_REPRESENTATION(#7704,#7611);
#7550=PROPERTY_DEFINITION_REPRESENTATION(#7705,#7612);
#7551=PROPERTY_DEFINITION_REPRESENTATION(#7706,#7613);
#7552=PROPERTY_DEFINITION_REPRESENTATION(#7707,#7614);
#7553=PROPERTY_DEFINITION_REPRESENTATION(#7708,#7615);
#7554=PROPERTY_DEFINITION_REPRESENTATION(#7709,#7616);
#7555=PROPERTY_DEFINITION_REPRESENTATION(#7710,#7617);
#7556=PROPERTY_DEFINITION_REPRESENTATION(#7711,#7618);
#7557=PROPERTY_DEFINITION_REPRESENTATION(#7712,#7619);
#7558=PROPERTY_DEFINITION_REPRESENTATION(#7713,#7620);
#7559=PROPERTY_DEFINITION_REPRESENTATION(#7714,#7621);
#7560=PROPERTY_DEFINITION_REPRESENTATION(#7715,#7622);
#7561=PROPERTY_DEFINITION_REPRESENTATION(#7716,#7623);
#7562=PROPERTY_DEFINITION_REPRESENTATION(#7717,#7624);
#7563=PROPERTY_DEFINITION_REPRESENTATION(#7718,#7625);
#7564=PROPERTY_DEFINITION_REPRESENTATION(#7719,#7626);
#7565=PROPERTY_DEFINITION_REPRESENTATION(#7720,#7627);
#7566=PROPERTY_DEFINITION_REPRESENTATION(#7721,#7628);
#7567=PROPERTY_DEFINITION_REPRESENTATION(#7722,#7629);
#7568=PROPERTY_DEFINITION_REPRESENTATION(#7723,#7630);
#7569=PROPERTY_DEFINITION_REPRESENTATION(#7724,#7631);
#7570=PROPERTY_DEFINITION_REPRESENTATION(#7725,#7632);
#7571=PROPERTY_DEFINITION_REPRESENTATION(#7726,#7633);
#7572=PROPERTY_DEFINITION_REPRESENTATION(#7727,#7634);
#7573=PROPERTY_DEFINITION_REPRESENTATION(#7728,#7635);
#7574=PROPERTY_DEFINITION_REPRESENTATION(#7729,#7636);
#7575=PROPERTY_DEFINITION_REPRESENTATION(#7730,#7637);
#7576=PROPERTY_DEFINITION_REPRESENTATION(#7731,#7638);
#7577=PROPERTY_DEFINITION_REPRESENTATION(#7732,#7639);
#7578=PROPERTY_DEFINITION_REPRESENTATION(#7733,#7640);
#7579=PROPERTY_DEFINITION_REPRESENTATION(#7734,#7641);
#7580=PROPERTY_DEFINITION_REPRESENTATION(#7735,#7642);
#7581=PROPERTY_DEFINITION_REPRESENTATION(#7736,#7643);
#7582=PROPERTY_DEFINITION_REPRESENTATION(#7737,#7644);
#7583=PROPERTY_DEFINITION_REPRESENTATION(#7738,#7645);
#7584=PROPERTY_DEFINITION_REPRESENTATION(#7739,#7646);
#7585=PROPERTY_DEFINITION_REPRESENTATION(#7740,#7647);
#7586=REPRESENTATION('material name',(#7648),#12771);
#7587=REPRESENTATION('density',(#7493),#12771);
#7588=REPRESENTATION('material name',(#7649),#12772);
#7589=REPRESENTATION('density',(#7494),#12772);
#7590=REPRESENTATION('material name',(#7650),#12773);
#7591=REPRESENTATION('density',(#7495),#12773);
#7592=REPRESENTATION('material name',(#7651),#12774);
#7593=REPRESENTATION('density',(#7496),#12774);
#7594=REPRESENTATION('material name',(#7652),#12775);
#7595=REPRESENTATION('density',(#7497),#12775);
#7596=REPRESENTATION('material name',(#7653),#12776);
#7597=REPRESENTATION('density',(#7498),#12776);
#7598=REPRESENTATION('material name',(#7654),#12777);
#7599=REPRESENTATION('density',(#7499),#12777);
#7600=REPRESENTATION('material name',(#7655),#12778);
#7601=REPRESENTATION('density',(#7500),#12778);
#7602=REPRESENTATION('material name',(#7656),#12779);
#7603=REPRESENTATION('density',(#7501),#12779);
#7604=REPRESENTATION('material name',(#7657),#12780);
#7605=REPRESENTATION('density',(#7502),#12780);
#7606=REPRESENTATION('material name',(#7658),#12781);
#7607=REPRESENTATION('density',(#7503),#12781);
#7608=REPRESENTATION('material name',(#7659),#12782);
#7609=REPRESENTATION('density',(#7504),#12782);
#7610=REPRESENTATION('material name',(#7660),#12783);
#7611=REPRESENTATION('density',(#7505),#12783);
#7612=REPRESENTATION('material name',(#7661),#12784);
#7613=REPRESENTATION('density',(#7506),#12784);
#7614=REPRESENTATION('material name',(#7662),#12785);
#7615=REPRESENTATION('density',(#7507),#12785);
#7616=REPRESENTATION('material name',(#7663),#12786);
#7617=REPRESENTATION('density',(#7508),#12786);
#7618=REPRESENTATION('material name',(#7664),#12787);
#7619=REPRESENTATION('density',(#7509),#12787);
#7620=REPRESENTATION('material name',(#7665),#12788);
#7621=REPRESENTATION('density',(#7510),#12788);
#7622=REPRESENTATION('material name',(#7666),#12789);
#7623=REPRESENTATION('density',(#7511),#12789);
#7624=REPRESENTATION('material name',(#7667),#12791);
#7625=REPRESENTATION('density',(#7512),#12791);
#7626=REPRESENTATION('material name',(#7668),#12792);
#7627=REPRESENTATION('density',(#7513),#12792);
#7628=REPRESENTATION('material name',(#7669),#12793);
#7629=REPRESENTATION('density',(#7514),#12793);
#7630=REPRESENTATION('material name',(#7670),#12795);
#7631=REPRESENTATION('density',(#7515),#12795);
#7632=REPRESENTATION('material name',(#7671),#12796);
#7633=REPRESENTATION('density',(#7516),#12796);
#7634=REPRESENTATION('material name',(#7672),#12797);
#7635=REPRESENTATION('density',(#7517),#12797);
#7636=REPRESENTATION('material name',(#7673),#12798);
#7637=REPRESENTATION('density',(#7518),#12798);
#7638=REPRESENTATION('material name',(#7674),#12799);
#7639=REPRESENTATION('density',(#7519),#12799);
#7640=REPRESENTATION('material name',(#7675),#12800);
#7641=REPRESENTATION('density',(#7520),#12800);
#7642=REPRESENTATION('material name',(#7676),#12801);
#7643=REPRESENTATION('density',(#7521),#12801);
#7644=REPRESENTATION('material name',(#7677),#12802);
#7645=REPRESENTATION('density',(#7522),#12802);
#7646=REPRESENTATION('material name',(#7678),#12803);
#7647=REPRESENTATION('density',(#7523),#12803);
#7648=DESCRIPTIVE_REPRESENTATION_ITEM('Steel','Steel');
#7649=DESCRIPTIVE_REPRESENTATION_ITEM('Steel','Steel');
#7650=DESCRIPTIVE_REPRESENTATION_ITEM('Steel','Steel');
#7651=DESCRIPTIVE_REPRESENTATION_ITEM('Steel','Steel');
#7652=DESCRIPTIVE_REPRESENTATION_ITEM('Steel','Steel');
#7653=DESCRIPTIVE_REPRESENTATION_ITEM('Steel','Steel');
#7654=DESCRIPTIVE_REPRESENTATION_ITEM('Steel','Steel');
#7655=DESCRIPTIVE_REPRESENTATION_ITEM('Steel','Steel');
#7656=DESCRIPTIVE_REPRESENTATION_ITEM('Steel','Steel');
#7657=DESCRIPTIVE_REPRESENTATION_ITEM('Steel','Steel');
#7658=DESCRIPTIVE_REPRESENTATION_ITEM('Steel','Steel');
#7659=DESCRIPTIVE_REPRESENTATION_ITEM('Steel','Steel');
#7660=DESCRIPTIVE_REPRESENTATION_ITEM('Steel','Steel');
#7661=DESCRIPTIVE_REPRESENTATION_ITEM('Steel','Steel');
#7662=DESCRIPTIVE_REPRESENTATION_ITEM('Steel','Steel');
#7663=DESCRIPTIVE_REPRESENTATION_ITEM('Steel','Steel');
#7664=DESCRIPTIVE_REPRESENTATION_ITEM('Steel','Steel');
#7665=DESCRIPTIVE_REPRESENTATION_ITEM('Steel','Steel');
#7666=DESCRIPTIVE_REPRESENTATION_ITEM('Steel','Steel');
#7667=DESCRIPTIVE_REPRESENTATION_ITEM('Steel','Steel');
#7668=DESCRIPTIVE_REPRESENTATION_ITEM('Steel','Steel');
#7669=DESCRIPTIVE_REPRESENTATION_ITEM('Steel','Steel');
#7670=DESCRIPTIVE_REPRESENTATION_ITEM('Steel','Steel');
#7671=DESCRIPTIVE_REPRESENTATION_ITEM('Steel','Steel');
#7672=DESCRIPTIVE_REPRESENTATION_ITEM('Steel','Steel');
#7673=DESCRIPTIVE_REPRESENTATION_ITEM('Steel','Steel');
#7674=DESCRIPTIVE_REPRESENTATION_ITEM('Steel','Steel');
#7675=DESCRIPTIVE_REPRESENTATION_ITEM('Steel','Steel');
#7676=DESCRIPTIVE_REPRESENTATION_ITEM('Steel','Steel');
#7677=DESCRIPTIVE_REPRESENTATION_ITEM('Steel','Steel');
#7678=DESCRIPTIVE_REPRESENTATION_ITEM('Steel','Steel');
#7679=PROPERTY_DEFINITION('material property','material name',#13037);
#7680=PROPERTY_DEFINITION('material property','density of part',#13037);
#7681=PROPERTY_DEFINITION('material property','material name',#13038);
#7682=PROPERTY_DEFINITION('material property','density of part',#13038);
#7683=PROPERTY_DEFINITION('material property','material name',#13039);
#7684=PROPERTY_DEFINITION('material property','density of part',#13039);
#7685=PROPERTY_DEFINITION('material property','material name',#13040);
#7686=PROPERTY_DEFINITION('material property','density of part',#13040);
#7687=PROPERTY_DEFINITION('material property','material name',#13041);
#7688=PROPERTY_DEFINITION('material property','density of part',#13041);
#7689=PROPERTY_DEFINITION('material property','material name',#13042);
#7690=PROPERTY_DEFINITION('material property','density of part',#13042);
#7691=PROPERTY_DEFINITION('material property','material name',#13043);
#7692=PROPERTY_DEFINITION('material property','density of part',#13043);
#7693=PROPERTY_DEFINITION('material property','material name',#13044);
#7694=PROPERTY_DEFINITION('material property','density of part',#13044);
#7695=PROPERTY_DEFINITION('material property','material name',#13045);
#7696=PROPERTY_DEFINITION('material property','density of part',#13045);
#7697=PROPERTY_DEFINITION('material property','material name',#13046);
#7698=PROPERTY_DEFINITION('material property','density of part',#13046);
#7699=PROPERTY_DEFINITION('material property','material name',#13047);
#7700=PROPERTY_DEFINITION('material property','density of part',#13047);
#7701=PROPERTY_DEFINITION('material property','material name',#13048);
#7702=PROPERTY_DEFINITION('material property','density of part',#13048);
#7703=PROPERTY_DEFINITION('material property','material name',#13049);
#7704=PROPERTY_DEFINITION('material property','density of part',#13049);
#7705=PROPERTY_DEFINITION('material property','material name',#13050);
#7706=PROPERTY_DEFINITION('material property','density of part',#13050);
#7707=PROPERTY_DEFINITION('material property','material name',#13051);
#7708=PROPERTY_DEFINITION('material property','density of part',#13051);
#7709=PROPERTY_DEFINITION('material property','material name',#13052);
#7710=PROPERTY_DEFINITION('material property','density of part',#13052);
#7711=PROPERTY_DEFINITION('material property','material name',#13053);
#7712=PROPERTY_DEFINITION('material property','density of part',#13053);
#7713=PROPERTY_DEFINITION('material property','material name',#13054);
#7714=PROPERTY_DEFINITION('material property','density of part',#13054);
#7715=PROPERTY_DEFINITION('material property','material name',#13055);
#7716=PROPERTY_DEFINITION('material property','density of part',#13055);
#7717=PROPERTY_DEFINITION('material property','material name',#13057);
#7718=PROPERTY_DEFINITION('material property','density of part',#13057);
#7719=PROPERTY_DEFINITION('material property','material name',#13058);
#7720=PROPERTY_DEFINITION('material property','density of part',#13058);
#7721=PROPERTY_DEFINITION('material property','material name',#13059);
#7722=PROPERTY_DEFINITION('material property','density of part',#13059);
#7723=PROPERTY_DEFINITION('material property','material name',#13061);
#7724=PROPERTY_DEFINITION('material property','density of part',#13061);
#7725=PROPERTY_DEFINITION('material property','material name',#13062);
#7726=PROPERTY_DEFINITION('material property','density of part',#13062);
#7727=PROPERTY_DEFINITION('material property','material name',#13063);
#7728=PROPERTY_DEFINITION('material property','density of part',#13063);
#7729=PROPERTY_DEFINITION('material property','material name',#13064);
#7730=PROPERTY_DEFINITION('material property','density of part',#13064);
#7731=PROPERTY_DEFINITION('material property','material name',#13065);
#7732=PROPERTY_DEFINITION('material property','density of part',#13065);
#7733=PROPERTY_DEFINITION('material property','material name',#13066);
#7734=PROPERTY_DEFINITION('material property','density of part',#13066);
#7735=PROPERTY_DEFINITION('material property','material name',#13067);
#7736=PROPERTY_DEFINITION('material property','density of part',#13067);
#7737=PROPERTY_DEFINITION('material property','material name',#13068);
#7738=PROPERTY_DEFINITION('material property','density of part',#13068);
#7739=PROPERTY_DEFINITION('material property','material name',#13069);
#7740=PROPERTY_DEFINITION('material property','density of part',#13069);
#7741=AXIS2_PLACEMENT_3D('',#10688,#8487,#8488);
#7742=AXIS2_PLACEMENT_3D('',#10689,#8489,#8490);
#7743=AXIS2_PLACEMENT_3D('',#10690,#8491,#8492);
#7744=AXIS2_PLACEMENT_3D('',#10691,#8493,#8494);
#7745=AXIS2_PLACEMENT_3D('',#10693,#8495,#8496);
#7746=AXIS2_PLACEMENT_3D('',#10696,#8498,#8499);
#7747=AXIS2_PLACEMENT_3D('',#10697,#8500,#8501);
#7748=AXIS2_PLACEMENT_3D('',#10699,#8502,#8503);
#7749=AXIS2_PLACEMENT_3D('',#10702,#8505,#8506);
#7750=AXIS2_PLACEMENT_3D('',#10703,#8507,#8508);
#7751=AXIS2_PLACEMENT_3D('',#10705,#8509,#8510);
#7752=AXIS2_PLACEMENT_3D('',#10708,#8512,#8513);
#7753=AXIS2_PLACEMENT_3D('',#10709,#8514,#8515);
#7754=AXIS2_PLACEMENT_3D('',#10711,#8516,#8517);
#7755=AXIS2_PLACEMENT_3D('',#10714,#8519,#8520);
#7756=AXIS2_PLACEMENT_3D('',#10715,#8521,#8522);
#7757=AXIS2_PLACEMENT_3D('',#10717,#8523,#8524);
#7758=AXIS2_PLACEMENT_3D('',#10720,#8526,#8527);
#7759=AXIS2_PLACEMENT_3D('',#10721,#8528,#8529);
#7760=AXIS2_PLACEMENT_3D('',#10723,#8530,#8531);
#7761=AXIS2_PLACEMENT_3D('',#10726,#8533,#8534);
#7762=AXIS2_PLACEMENT_3D('',#10727,#8535,#8536);
#7763=AXIS2_PLACEMENT_3D('',#10736,#8541,#8542);
#7764=AXIS2_PLACEMENT_3D('',#10742,#8546,#8547);
#7765=AXIS2_PLACEMENT_3D('',#10748,#8551,#8552);
#7766=AXIS2_PLACEMENT_3D('',#10751,#8555,#8556);
#7767=AXIS2_PLACEMENT_3D('',#10752,#8557,#8558);
#7768=AXIS2_PLACEMENT_3D('',#10753,#8559,#8560);
#7769=AXIS2_PLACEMENT_3D('',#10754,#8561,#8562);
#7770=AXIS2_PLACEMENT_3D('',#10756,#8563,#8564);
#7771=AXIS2_PLACEMENT_3D('',#10759,#8566,#8567);
#7772=AXIS2_PLACEMENT_3D('',#10760,#8568,#8569);
#7773=AXIS2_PLACEMENT_3D('',#10762,#8570,#8571);
#7774=AXIS2_PLACEMENT_3D('',#10765,#8573,#8574);
#7775=AXIS2_PLACEMENT_3D('',#10766,#8575,#8576);
#7776=AXIS2_PLACEMENT_3D('',#10768,#8577,#8578);
#7777=AXIS2_PLACEMENT_3D('',#10771,#8580,#8581);
#7778=AXIS2_PLACEMENT_3D('',#10772,#8582,#8583);
#7779=AXIS2_PLACEMENT_3D('',#10774,#8584,#8585);
#7780=AXIS2_PLACEMENT_3D('',#10777,#8587,#8588);
#7781=AXIS2_PLACEMENT_3D('',#10778,#8589,#8590);
#7782=AXIS2_PLACEMENT_3D('',#10780,#8591,#8592);
#7783=AXIS2_PLACEMENT_3D('',#10783,#8594,#8595);
#7784=AXIS2_PLACEMENT_3D('',#10784,#8596,#8597);
#7785=AXIS2_PLACEMENT_3D('',#10786,#8598,#8599);
#7786=AXIS2_PLACEMENT_3D('',#10789,#8601,#8602);
#7787=AXIS2_PLACEMENT_3D('',#10790,#8603,#8604);
#7788=AXIS2_PLACEMENT_3D('',#10799,#8609,#8610);
#7789=AXIS2_PLACEMENT_3D('',#10805,#8614,#8615);
#7790=AXIS2_PLACEMENT_3D('',#10811,#8619,#8620);
#7791=AXIS2_PLACEMENT_3D('',#10814,#8623,#8624);
#7792=AXIS2_PLACEMENT_3D('',#10815,#8625,#8626);
#7793=AXIS2_PLACEMENT_3D('',#10816,#8627,#8628);
#7794=AXIS2_PLACEMENT_3D('',#10817,#8629,#8630);
#7795=AXIS2_PLACEMENT_3D('',#10819,#8631,#8632);
#7796=AXIS2_PLACEMENT_3D('',#10822,#8634,#8635);
#7797=AXIS2_PLACEMENT_3D('',#10823,#8636,#8637);
#7798=AXIS2_PLACEMENT_3D('',#10825,#8638,#8639);
#7799=AXIS2_PLACEMENT_3D('',#10828,#8641,#8642);
#7800=AXIS2_PLACEMENT_3D('',#10829,#8643,#8644);
#7801=AXIS2_PLACEMENT_3D('',#10838,#8649,#8650);
#7802=AXIS2_PLACEMENT_3D('',#10844,#8654,#8655);
#7803=AXIS2_PLACEMENT_3D('',#10850,#8659,#8660);
#7804=AXIS2_PLACEMENT_3D('',#10853,#8663,#8664);
#7805=AXIS2_PLACEMENT_3D('',#10854,#8665,#8666);
#7806=AXIS2_PLACEMENT_3D('',#10855,#8667,#8668);
#7807=AXIS2_PLACEMENT_3D('',#10856,#8669,#8670);
#7808=AXIS2_PLACEMENT_3D('',#10858,#8671,#8672);
#7809=AXIS2_PLACEMENT_3D('',#10861,#8674,#8675);
#7810=AXIS2_PLACEMENT_3D('',#10862,#8676,#8677);
#7811=AXIS2_PLACEMENT_3D('',#10864,#8678,#8679);
#7812=AXIS2_PLACEMENT_3D('',#10867,#8681,#8682);
#7813=AXIS2_PLACEMENT_3D('',#10868,#8683,#8684);
#7814=AXIS2_PLACEMENT_3D('',#10877,#8689,#8690);
#7815=AXIS2_PLACEMENT_3D('',#10883,#8694,#8695);
#7816=AXIS2_PLACEMENT_3D('',#10889,#8699,#8700);
#7817=AXIS2_PLACEMENT_3D('',#10892,#8703,#8704);
#7818=AXIS2_PLACEMENT_3D('',#10893,#8705,#8706);
#7819=AXIS2_PLACEMENT_3D('',#10894,#8707,#8708);
#7820=AXIS2_PLACEMENT_3D('',#10895,#8709,#8710);
#7821=AXIS2_PLACEMENT_3D('',#10904,#8715,#8716);
#7822=AXIS2_PLACEMENT_3D('',#10910,#8720,#8721);
#7823=AXIS2_PLACEMENT_3D('',#10916,#8725,#8726);
#7824=AXIS2_PLACEMENT_3D('',#10919,#8729,#8730);
#7825=AXIS2_PLACEMENT_3D('',#10920,#8731,#8732);
#7826=AXIS2_PLACEMENT_3D('',#10921,#8733,#8734);
#7827=AXIS2_PLACEMENT_3D('',#10922,#8735,#8736);
#7828=AXIS2_PLACEMENT_3D('',#10931,#8741,#8742);
#7829=AXIS2_PLACEMENT_3D('',#10937,#8746,#8747);
#7830=AXIS2_PLACEMENT_3D('',#10943,#8751,#8752);
#7831=AXIS2_PLACEMENT_3D('',#10946,#8755,#8756);
#7832=AXIS2_PLACEMENT_3D('',#10947,#8757,#8758);
#7833=AXIS2_PLACEMENT_3D('',#10948,#8759,#8760);
#7834=AXIS2_PLACEMENT_3D('',#10949,#8761,#8762);
#7835=AXIS2_PLACEMENT_3D('',#10951,#8763,#8764);
#7836=AXIS2_PLACEMENT_3D('',#10954,#8766,#8767);
#7837=AXIS2_PLACEMENT_3D('',#10955,#8768,#8769);
#7838=AXIS2_PLACEMENT_3D('',#10957,#8770,#8771);
#7839=AXIS2_PLACEMENT_3D('',#10960,#8773,#8774);
#7840=AXIS2_PLACEMENT_3D('',#10961,#8775,#8776);
#7841=AXIS2_PLACEMENT_3D('',#10970,#8781,#8782);
#7842=AXIS2_PLACEMENT_3D('',#10976,#8786,#8787);
#7843=AXIS2_PLACEMENT_3D('',#10982,#8791,#8792);
#7844=AXIS2_PLACEMENT_3D('',#10985,#8795,#8796);
#7845=AXIS2_PLACEMENT_3D('',#10986,#8797,#8798);
#7846=AXIS2_PLACEMENT_3D('',#10987,#8799,#8800);
#7847=AXIS2_PLACEMENT_3D('',#10988,#8801,#8802);
#7848=AXIS2_PLACEMENT_3D('',#10990,#8803,#8804);
#7849=AXIS2_PLACEMENT_3D('',#10993,#8806,#8807);
#7850=AXIS2_PLACEMENT_3D('',#10994,#8808,#8809);
#7851=AXIS2_PLACEMENT_3D('',#10996,#8810,#8811);
#7852=AXIS2_PLACEMENT_3D('',#10999,#8813,#8814);
#7853=AXIS2_PLACEMENT_3D('',#11000,#8815,#8816);
#7854=AXIS2_PLACEMENT_3D('',#11009,#8821,#8822);
#7855=AXIS2_PLACEMENT_3D('',#11015,#8826,#8827);
#7856=AXIS2_PLACEMENT_3D('',#11021,#8831,#8832);
#7857=AXIS2_PLACEMENT_3D('',#11024,#8835,#8836);
#7858=AXIS2_PLACEMENT_3D('',#11025,#8837,#8838);
#7859=AXIS2_PLACEMENT_3D('',#11026,#8839,#8840);
#7860=AXIS2_PLACEMENT_3D('',#11027,#8841,#8842);
#7861=AXIS2_PLACEMENT_3D('',#11036,#8847,#8848);
#7862=AXIS2_PLACEMENT_3D('',#11042,#8852,#8853);
#7863=AXIS2_PLACEMENT_3D('',#11048,#8857,#8858);
#7864=AXIS2_PLACEMENT_3D('',#11051,#8861,#8862);
#7865=AXIS2_PLACEMENT_3D('',#11052,#8863,#8864);
#7866=AXIS2_PLACEMENT_3D('',#11053,#8865,#8866);
#7867=AXIS2_PLACEMENT_3D('',#11054,#8867,#8868);
#7868=AXIS2_PLACEMENT_3D('',#11063,#8873,#8874);
#7869=AXIS2_PLACEMENT_3D('',#11069,#8878,#8879);
#7870=AXIS2_PLACEMENT_3D('',#11075,#8883,#8884);
#7871=AXIS2_PLACEMENT_3D('',#11078,#8887,#8888);
#7872=AXIS2_PLACEMENT_3D('',#11079,#8889,#8890);
#7873=AXIS2_PLACEMENT_3D('',#11080,#8891,#8892);
#7874=AXIS2_PLACEMENT_3D('',#11081,#8893,#8894);
#7875=AXIS2_PLACEMENT_3D('',#11086,#8896,#8897);
#7876=AXIS2_PLACEMENT_3D('',#11089,#8899,#8900);
#7877=AXIS2_PLACEMENT_3D('',#11090,#8901,#8902);
#7878=AXIS2_PLACEMENT_3D('',#11092,#8904,#8905);
#7879=AXIS2_PLACEMENT_3D('',#11094,#8907,#8908);
#7880=AXIS2_PLACEMENT_3D('',#11095,#8909,#8910);
#7881=AXIS2_PLACEMENT_3D('',#11097,#8911,#8912);
#7882=AXIS2_PLACEMENT_3D('',#11098,#8913,#8914);
#7883=AXIS2_PLACEMENT_3D('',#11103,#8916,#8917);
#7884=AXIS2_PLACEMENT_3D('',#11106,#8919,#8920);
#7885=AXIS2_PLACEMENT_3D('',#11107,#8921,#8922);
#7886=AXIS2_PLACEMENT_3D('',#11109,#8924,#8925);
#7887=AXIS2_PLACEMENT_3D('',#11111,#8927,#8928);
#7888=AXIS2_PLACEMENT_3D('',#11112,#8929,#8930);
#7889=AXIS2_PLACEMENT_3D('',#11114,#8931,#8932);
#7890=AXIS2_PLACEMENT_3D('',#11115,#8933,#8934);
#7891=AXIS2_PLACEMENT_3D('',#11121,#8938,#8939);
#7892=AXIS2_PLACEMENT_3D('',#11124,#8942,#8943);
#7893=AXIS2_PLACEMENT_3D('',#11130,#8947,#8948);
#7894=AXIS2_PLACEMENT_3D('',#11132,#8949,#8950);
#7895=AXIS2_PLACEMENT_3D('',#11134,#8952,#8953);
#7896=AXIS2_PLACEMENT_3D('',#11136,#8954,#8955);
#7897=AXIS2_PLACEMENT_3D('',#11138,#8957,#8958);
#7898=AXIS2_PLACEMENT_3D('',#11144,#8962,#8963);
#7899=AXIS2_PLACEMENT_3D('',#11148,#8966,#8967);
#7900=AXIS2_PLACEMENT_3D('',#11152,#8970,#8971);
#7901=AXIS2_PLACEMENT_3D('',#11154,#8973,#8974);
#7902=AXIS2_PLACEMENT_3D('',#11155,#8975,#8976);
#7903=AXIS2_PLACEMENT_3D('',#11156,#8977,#8978);
#7904=AXIS2_PLACEMENT_3D('',#11165,#8983,#8984);
#7905=AXIS2_PLACEMENT_3D('',#11171,#8988,#8989);
#7906=AXIS2_PLACEMENT_3D('',#11177,#8993,#8994);
#7907=AXIS2_PLACEMENT_3D('',#11180,#8997,#8998);
#7908=AXIS2_PLACEMENT_3D('',#11181,#8999,#9000);
#7909=AXIS2_PLACEMENT_3D('',#11182,#9001,#9002);
#7910=AXIS2_PLACEMENT_3D('',#11183,#9003,#9004);
#7911=AXIS2_PLACEMENT_3D('',#11188,#9006,#9007);
#7912=AXIS2_PLACEMENT_3D('',#11191,#9009,#9010);
#7913=AXIS2_PLACEMENT_3D('',#11192,#9011,#9012);
#7914=AXIS2_PLACEMENT_3D('',#11194,#9014,#9015);
#7915=AXIS2_PLACEMENT_3D('',#11196,#9017,#9018);
#7916=AXIS2_PLACEMENT_3D('',#11197,#9019,#9020);
#7917=AXIS2_PLACEMENT_3D('',#11199,#9021,#9022);
#7918=AXIS2_PLACEMENT_3D('',#11200,#9023,#9024);
#7919=AXIS2_PLACEMENT_3D('',#11205,#9026,#9027);
#7920=AXIS2_PLACEMENT_3D('',#11208,#9029,#9030);
#7921=AXIS2_PLACEMENT_3D('',#11209,#9031,#9032);
#7922=AXIS2_PLACEMENT_3D('',#11211,#9034,#9035);
#7923=AXIS2_PLACEMENT_3D('',#11213,#9037,#9038);
#7924=AXIS2_PLACEMENT_3D('',#11214,#9039,#9040);
#7925=AXIS2_PLACEMENT_3D('',#11216,#9041,#9042);
#7926=AXIS2_PLACEMENT_3D('',#11217,#9043,#9044);
#7927=AXIS2_PLACEMENT_3D('',#11223,#9048,#9049);
#7928=AXIS2_PLACEMENT_3D('',#11226,#9052,#9053);
#7929=AXIS2_PLACEMENT_3D('',#11232,#9057,#9058);
#7930=AXIS2_PLACEMENT_3D('',#11234,#9059,#9060);
#7931=AXIS2_PLACEMENT_3D('',#11236,#9062,#9063);
#7932=AXIS2_PLACEMENT_3D('',#11238,#9064,#9065);
#7933=AXIS2_PLACEMENT_3D('',#11240,#9067,#9068);
#7934=AXIS2_PLACEMENT_3D('',#11246,#9072,#9073);
#7935=AXIS2_PLACEMENT_3D('',#11250,#9076,#9077);
#7936=AXIS2_PLACEMENT_3D('',#11254,#9080,#9081);
#7937=AXIS2_PLACEMENT_3D('',#11256,#9083,#9084);
#7938=AXIS2_PLACEMENT_3D('',#11257,#9085,#9086);
#7939=AXIS2_PLACEMENT_3D('',#11258,#9087,#9088);
#7940=AXIS2_PLACEMENT_3D('',#11267,#9093,#9094);
#7941=AXIS2_PLACEMENT_3D('',#11273,#9098,#9099);
#7942=AXIS2_PLACEMENT_3D('',#11279,#9103,#9104);
#7943=AXIS2_PLACEMENT_3D('',#11282,#9107,#9108);
#7944=AXIS2_PLACEMENT_3D('',#11283,#9109,#9110);
#7945=AXIS2_PLACEMENT_3D('',#11284,#9111,#9112);
#7946=AXIS2_PLACEMENT_3D('',#11285,#9113,#9114);
#7947=AXIS2_PLACEMENT_3D('',#11294,#9119,#9120);
#7948=AXIS2_PLACEMENT_3D('',#11300,#9124,#9125);
#7949=AXIS2_PLACEMENT_3D('',#11306,#9129,#9130);
#7950=AXIS2_PLACEMENT_3D('',#11312,#9134,#9135);
#7951=AXIS2_PLACEMENT_3D('',#11318,#9139,#9140);
#7952=AXIS2_PLACEMENT_3D('',#11324,#9144,#9145);
#7953=AXIS2_PLACEMENT_3D('',#11330,#9149,#9150);
#7954=AXIS2_PLACEMENT_3D('',#11336,#9154,#9155);
#7955=AXIS2_PLACEMENT_3D('',#11342,#9159,#9160);
#7956=AXIS2_PLACEMENT_3D('',#11351,#9165,#9166);
#7957=AXIS2_PLACEMENT_3D('',#11357,#9170,#9171);
#7958=AXIS2_PLACEMENT_3D('',#11363,#9175,#9176);
#7959=AXIS2_PLACEMENT_3D('',#11369,#9180,#9181);
#7960=AXIS2_PLACEMENT_3D('',#11375,#9185,#9186);
#7961=AXIS2_PLACEMENT_3D('',#11381,#9190,#9191);
#7962=AXIS2_PLACEMENT_3D('',#11387,#9195,#9196);
#7963=AXIS2_PLACEMENT_3D('',#11393,#9200,#9201);
#7964=AXIS2_PLACEMENT_3D('',#11399,#9205,#9206);
#7965=AXIS2_PLACEMENT_3D('',#11408,#9211,#9212);
#7966=AXIS2_PLACEMENT_3D('',#11414,#9216,#9217);
#7967=AXIS2_PLACEMENT_3D('',#11420,#9221,#9222);
#7968=AXIS2_PLACEMENT_3D('',#11426,#9226,#9227);
#7969=AXIS2_PLACEMENT_3D('',#11432,#9231,#9232);
#7970=AXIS2_PLACEMENT_3D('',#11438,#9236,#9237);
#7971=AXIS2_PLACEMENT_3D('',#11444,#9241,#9242);
#7972=AXIS2_PLACEMENT_3D('',#11450,#9246,#9247);
#7973=AXIS2_PLACEMENT_3D('',#11456,#9251,#9252);
#7974=AXIS2_PLACEMENT_3D('',#11465,#9257,#9258);
#7975=AXIS2_PLACEMENT_3D('',#11471,#9262,#9263);
#7976=AXIS2_PLACEMENT_3D('',#11477,#9267,#9268);
#7977=AXIS2_PLACEMENT_3D('',#11483,#9272,#9273);
#7978=AXIS2_PLACEMENT_3D('',#11489,#9277,#9278);
#7979=AXIS2_PLACEMENT_3D('',#11495,#9282,#9283);
#7980=AXIS2_PLACEMENT_3D('',#11501,#9287,#9288);
#7981=AXIS2_PLACEMENT_3D('',#11507,#9292,#9293);
#7982=AXIS2_PLACEMENT_3D('',#11513,#9297,#9298);
#7983=AXIS2_PLACEMENT_3D('',#11515,#9299,#9300);
#7984=AXIS2_PLACEMENT_3D('',#11518,#9302,#9303);
#7985=AXIS2_PLACEMENT_3D('',#11519,#9304,#9305);
#7986=AXIS2_PLACEMENT_3D('',#11525,#9309,#9310);
#7987=AXIS2_PLACEMENT_3D('',#11531,#9314,#9315);
#7988=AXIS2_PLACEMENT_3D('',#11534,#9318,#9319);
#7989=AXIS2_PLACEMENT_3D('',#11540,#9323,#9324);
#7990=AXIS2_PLACEMENT_3D('',#11543,#9327,#9328);
#7991=AXIS2_PLACEMENT_3D('',#11549,#9332,#9333);
#7992=AXIS2_PLACEMENT_3D('',#11552,#9336,#9337);
#7993=AXIS2_PLACEMENT_3D('',#11555,#9340,#9341);
#7994=AXIS2_PLACEMENT_3D('',#11556,#9342,#9343);
#7995=AXIS2_PLACEMENT_3D('',#11557,#9344,#9345);
#7996=AXIS2_PLACEMENT_3D('',#11558,#9346,#9347);
#7997=AXIS2_PLACEMENT_3D('',#11560,#9348,#9349);
#7998=AXIS2_PLACEMENT_3D('',#11563,#9351,#9352);
#7999=AXIS2_PLACEMENT_3D('',#11564,#9353,#9354);
#8000=AXIS2_PLACEMENT_3D('',#11566,#9355,#9356);
#8001=AXIS2_PLACEMENT_3D('',#11567,#9357,#9358);
#8002=AXIS2_PLACEMENT_3D('',#11569,#9359,#9360);
#8003=AXIS2_PLACEMENT_3D('',#11572,#9362,#9363);
#8004=AXIS2_PLACEMENT_3D('',#11573,#9364,#9365);
#8005=AXIS2_PLACEMENT_3D('',#11575,#9366,#9367);
#8006=AXIS2_PLACEMENT_3D('',#11576,#9368,#9369);
#8007=AXIS2_PLACEMENT_3D('',#11578,#9370,#9371);
#8008=AXIS2_PLACEMENT_3D('',#11581,#9373,#9374);
#8009=AXIS2_PLACEMENT_3D('',#11582,#9375,#9376);
#8010=AXIS2_PLACEMENT_3D('',#11584,#9377,#9378);
#8011=AXIS2_PLACEMENT_3D('',#11585,#9379,#9380);
#8012=AXIS2_PLACEMENT_3D('',#11587,#9381,#9382);
#8013=AXIS2_PLACEMENT_3D('',#11590,#9384,#9385);
#8014=AXIS2_PLACEMENT_3D('',#11591,#9386,#9387);
#8015=AXIS2_PLACEMENT_3D('',#11593,#9388,#9389);
#8016=AXIS2_PLACEMENT_3D('',#11594,#9390,#9391);
#8017=AXIS2_PLACEMENT_3D('',#11596,#9392,#9393);
#8018=AXIS2_PLACEMENT_3D('',#11598,#9395,#9396);
#8019=AXIS2_PLACEMENT_3D('',#11600,#9397,#9398);
#8020=AXIS2_PLACEMENT_3D('',#11602,#9400,#9401);
#8021=AXIS2_PLACEMENT_3D('',#11604,#9402,#9403);
#8022=AXIS2_PLACEMENT_3D('',#11606,#9405,#9406);
#8023=AXIS2_PLACEMENT_3D('',#11608,#9407,#9408);
#8024=AXIS2_PLACEMENT_3D('',#11610,#9410,#9411);
#8025=AXIS2_PLACEMENT_3D('',#11619,#9416,#9417);
#8026=AXIS2_PLACEMENT_3D('',#11625,#9421,#9422);
#8027=AXIS2_PLACEMENT_3D('',#11631,#9426,#9427);
#8028=AXIS2_PLACEMENT_3D('',#11637,#9431,#9432);
#8029=AXIS2_PLACEMENT_3D('',#11643,#9436,#9437);
#8030=AXIS2_PLACEMENT_3D('',#11649,#9441,#9442);
#8031=AXIS2_PLACEMENT_3D('',#11655,#9446,#9447);
#8032=AXIS2_PLACEMENT_3D('',#11661,#9451,#9452);
#8033=AXIS2_PLACEMENT_3D('',#11667,#9456,#9457);
#8034=AXIS2_PLACEMENT_3D('',#11673,#9461,#9462);
#8035=AXIS2_PLACEMENT_3D('',#11679,#9466,#9467);
#8036=AXIS2_PLACEMENT_3D('',#11682,#9470,#9471);
#8037=AXIS2_PLACEMENT_3D('',#11683,#9472,#9473);
#8038=AXIS2_PLACEMENT_3D('',#11684,#9474,#9475);
#8039=AXIS2_PLACEMENT_3D('',#11685,#9476,#9477);
#8040=AXIS2_PLACEMENT_3D('',#11687,#9478,#9479);
#8041=AXIS2_PLACEMENT_3D('',#11688,#9480,#9481);
#8042=AXIS2_PLACEMENT_3D('',#11690,#9482,#9483);
#8043=AXIS2_PLACEMENT_3D('',#11692,#9485,#9486);
#8044=AXIS2_PLACEMENT_3D('',#11694,#9487,#9488);
#8045=AXIS2_PLACEMENT_3D('',#11696,#9490,#9491);
#8046=AXIS2_PLACEMENT_3D('',#11698,#9492,#9493);
#8047=AXIS2_PLACEMENT_3D('',#11700,#9495,#9496);
#8048=AXIS2_PLACEMENT_3D('',#11702,#9497,#9498);
#8049=AXIS2_PLACEMENT_3D('',#11703,#9499,#9500);
#8050=AXIS2_PLACEMENT_3D('',#11705,#9501,#9502);
#8051=AXIS2_PLACEMENT_3D('',#11707,#9504,#9505);
#8052=AXIS2_PLACEMENT_3D('',#11709,#9506,#9507);
#8053=AXIS2_PLACEMENT_3D('',#11711,#9509,#9510);
#8054=AXIS2_PLACEMENT_3D('',#11713,#9511,#9512);
#8055=AXIS2_PLACEMENT_3D('',#11715,#9514,#9515);
#8056=AXIS2_PLACEMENT_3D('',#11716,#9516,#9517);
#8057=AXIS2_PLACEMENT_3D('',#11725,#9522,#9523);
#8058=AXIS2_PLACEMENT_3D('',#11731,#9527,#9528);
#8059=AXIS2_PLACEMENT_3D('',#11737,#9532,#9533);
#8060=AXIS2_PLACEMENT_3D('',#11743,#9537,#9538);
#8061=AXIS2_PLACEMENT_3D('',#11749,#9542,#9543);
#8062=AXIS2_PLACEMENT_3D('',#11752,#9546,#9547);
#8063=AXIS2_PLACEMENT_3D('',#11753,#9548,#9549);
#8064=AXIS2_PLACEMENT_3D('',#11754,#9550,#9551);
#8065=AXIS2_PLACEMENT_3D('',#11755,#9552,#9553);
#8066=AXIS2_PLACEMENT_3D('',#11764,#9558,#9559);
#8067=AXIS2_PLACEMENT_3D('',#11770,#9563,#9564);
#8068=AXIS2_PLACEMENT_3D('',#11777,#9568,#9569);
#8069=AXIS2_PLACEMENT_3D('',#11778,#9570,#9571);
#8070=AXIS2_PLACEMENT_3D('',#11792,#9579,#9580);
#8071=AXIS2_PLACEMENT_3D('',#11796,#9583,#9584);
#8072=AXIS2_PLACEMENT_3D('',#11800,#9587,#9588);
#8073=AXIS2_PLACEMENT_3D('',#11810,#9594,#9595);
#8074=AXIS2_PLACEMENT_3D('',#11812,#9597,#9598);
#8075=AXIS2_PLACEMENT_3D('',#11816,#9600,#9601);
#8076=AXIS2_PLACEMENT_3D('',#11818,#9603,#9604);
#8077=AXIS2_PLACEMENT_3D('',#11820,#9605,#9606);
#8078=AXIS2_PLACEMENT_3D('',#11823,#9608,#9609);
#8079=AXIS2_PLACEMENT_3D('',#11825,#9610,#9611);
#8080=AXIS2_PLACEMENT_3D('',#11826,#9612,#9613);
#8081=AXIS2_PLACEMENT_3D('',#11827,#9614,#9615);
#8082=AXIS2_PLACEMENT_3D('',#11829,#9617,#9618);
#8083=AXIS2_PLACEMENT_3D('',#11831,#9620,#9621);
#8084=AXIS2_PLACEMENT_3D('',#11833,#9623,#9624);
#8085=AXIS2_PLACEMENT_3D('',#11834,#9625,#9626);
#8086=AXIS2_PLACEMENT_3D('',#11835,#9627,#9628);
#8087=AXIS2_PLACEMENT_3D('',#11844,#9633,#9634);
#8088=AXIS2_PLACEMENT_3D('',#11850,#9638,#9639);
#8089=AXIS2_PLACEMENT_3D('',#11856,#9643,#9644);
#8090=AXIS2_PLACEMENT_3D('',#11862,#9648,#9649);
#8091=AXIS2_PLACEMENT_3D('',#11868,#9653,#9654);
#8092=AXIS2_PLACEMENT_3D('',#11871,#9657,#9658);
#8093=AXIS2_PLACEMENT_3D('',#11872,#9659,#9660);
#8094=AXIS2_PLACEMENT_3D('',#11873,#9661,#9662);
#8095=AXIS2_PLACEMENT_3D('',#11875,#9663,#9664);
#8096=AXIS2_PLACEMENT_3D('',#11876,#9665,#9666);
#8097=AXIS2_PLACEMENT_3D('',#11878,#9667,#9668);
#8098=AXIS2_PLACEMENT_3D('',#11879,#9669,#9670);
#8099=AXIS2_PLACEMENT_3D('',#11881,#9671,#9672);
#8100=AXIS2_PLACEMENT_3D('',#11883,#9674,#9675);
#8101=AXIS2_PLACEMENT_3D('',#11885,#9676,#9677);
#8102=AXIS2_PLACEMENT_3D('',#11887,#9679,#9680);
#8103=AXIS2_PLACEMENT_3D('',#11889,#9681,#9682);
#8104=AXIS2_PLACEMENT_3D('',#11891,#9684,#9685);
#8105=AXIS2_PLACEMENT_3D('',#11893,#9686,#9687);
#8106=AXIS2_PLACEMENT_3D('',#11894,#9688,#9689);
#8107=AXIS2_PLACEMENT_3D('',#11896,#9690,#9691);
#8108=AXIS2_PLACEMENT_3D('',#11898,#9693,#9694);
#8109=AXIS2_PLACEMENT_3D('',#11900,#9696,#9697);
#8110=AXIS2_PLACEMENT_3D('',#11901,#9698,#9699);
#8111=AXIS2_PLACEMENT_3D('',#11902,#9700,#9701);
#8112=AXIS2_PLACEMENT_3D('',#11904,#9702,#9703);
#8113=AXIS2_PLACEMENT_3D('',#11907,#9705,#9706);
#8114=AXIS2_PLACEMENT_3D('',#11908,#9707,#9708);
#8115=AXIS2_PLACEMENT_3D('',#11910,#9709,#9710);
#8116=AXIS2_PLACEMENT_3D('',#11913,#9712,#9713);
#8117=AXIS2_PLACEMENT_3D('',#11914,#9714,#9715);
#8118=AXIS2_PLACEMENT_3D('',#11916,#9716,#9717);
#8119=AXIS2_PLACEMENT_3D('',#11919,#9719,#9720);
#8120=AXIS2_PLACEMENT_3D('',#11920,#9721,#9722);
#8121=AXIS2_PLACEMENT_3D('',#11922,#9723,#9724);
#8122=AXIS2_PLACEMENT_3D('',#11925,#9726,#9727);
#8123=AXIS2_PLACEMENT_3D('',#11926,#9728,#9729);
#8124=AXIS2_PLACEMENT_3D('',#11928,#9730,#9731);
#8125=AXIS2_PLACEMENT_3D('',#11931,#9733,#9734);
#8126=AXIS2_PLACEMENT_3D('',#11932,#9735,#9736);
#8127=AXIS2_PLACEMENT_3D('',#11934,#9737,#9738);
#8128=AXIS2_PLACEMENT_3D('',#11937,#9740,#9741);
#8129=AXIS2_PLACEMENT_3D('',#11938,#9742,#9743);
#8130=AXIS2_PLACEMENT_3D('',#11940,#9744,#9745);
#8131=AXIS2_PLACEMENT_3D('',#11943,#9747,#9748);
#8132=AXIS2_PLACEMENT_3D('',#11944,#9749,#9750);
#8133=AXIS2_PLACEMENT_3D('',#11946,#9751,#9752);
#8134=AXIS2_PLACEMENT_3D('',#11949,#9754,#9755);
#8135=AXIS2_PLACEMENT_3D('',#11950,#9756,#9757);
#8136=AXIS2_PLACEMENT_3D('',#11952,#9758,#9759);
#8137=AXIS2_PLACEMENT_3D('',#11955,#9761,#9762);
#8138=AXIS2_PLACEMENT_3D('',#11956,#9763,#9764);
#8139=AXIS2_PLACEMENT_3D('',#11958,#9765,#9766);
#8140=AXIS2_PLACEMENT_3D('',#11961,#9768,#9769);
#8141=AXIS2_PLACEMENT_3D('',#11962,#9770,#9771);
#8142=AXIS2_PLACEMENT_3D('',#11964,#9772,#9773);
#8143=AXIS2_PLACEMENT_3D('',#11967,#9775,#9776);
#8144=AXIS2_PLACEMENT_3D('',#11968,#9777,#9778);
#8145=AXIS2_PLACEMENT_3D('',#11970,#9779,#9780);
#8146=AXIS2_PLACEMENT_3D('',#11973,#9782,#9783);
#8147=AXIS2_PLACEMENT_3D('',#11974,#9784,#9785);
#8148=AXIS2_PLACEMENT_3D('',#11976,#9786,#9787);
#8149=AXIS2_PLACEMENT_3D('',#11979,#9789,#9790);
#8150=AXIS2_PLACEMENT_3D('',#11980,#9791,#9792);
#8151=AXIS2_PLACEMENT_3D('',#11982,#9793,#9794);
#8152=AXIS2_PLACEMENT_3D('',#11985,#9796,#9797);
#8153=AXIS2_PLACEMENT_3D('',#11986,#9798,#9799);
#8154=AXIS2_PLACEMENT_3D('',#11988,#9800,#9801);
#8155=AXIS2_PLACEMENT_3D('',#11991,#9803,#9804);
#8156=AXIS2_PLACEMENT_3D('',#11992,#9805,#9806);
#8157=AXIS2_PLACEMENT_3D('',#11994,#9807,#9808);
#8158=AXIS2_PLACEMENT_3D('',#11997,#9810,#9811);
#8159=AXIS2_PLACEMENT_3D('',#11998,#9812,#9813);
#8160=AXIS2_PLACEMENT_3D('',#12000,#9814,#9815);
#8161=AXIS2_PLACEMENT_3D('',#12003,#9817,#9818);
#8162=AXIS2_PLACEMENT_3D('',#12004,#9819,#9820);
#8163=AXIS2_PLACEMENT_3D('',#12006,#9821,#9822);
#8164=AXIS2_PLACEMENT_3D('',#12009,#9824,#9825);
#8165=AXIS2_PLACEMENT_3D('',#12010,#9826,#9827);
#8166=AXIS2_PLACEMENT_3D('',#12012,#9828,#9829);
#8167=AXIS2_PLACEMENT_3D('',#12015,#9831,#9832);
#8168=AXIS2_PLACEMENT_3D('',#12016,#9833,#9834);
#8169=AXIS2_PLACEMENT_3D('',#12025,#9839,#9840);
#8170=AXIS2_PLACEMENT_3D('',#12031,#9844,#9845);
#8171=AXIS2_PLACEMENT_3D('',#12037,#9849,#9850);
#8172=AXIS2_PLACEMENT_3D('',#12040,#9853,#9854);
#8173=AXIS2_PLACEMENT_3D('',#12041,#9855,#9856);
#8174=AXIS2_PLACEMENT_3D('',#12042,#9857,#9858);
#8175=AXIS2_PLACEMENT_3D('',#12043,#9859,#9860);
#8176=AXIS2_PLACEMENT_3D('',#12045,#9861,#9862);
#8177=AXIS2_PLACEMENT_3D('',#12048,#9864,#9865);
#8178=AXIS2_PLACEMENT_3D('',#12049,#9866,#9867);
#8179=AXIS2_PLACEMENT_3D('',#12051,#9868,#9869);
#8180=AXIS2_PLACEMENT_3D('',#12054,#9871,#9872);
#8181=AXIS2_PLACEMENT_3D('',#12055,#9873,#9874);
#8182=AXIS2_PLACEMENT_3D('',#12056,#9875,#9876);
#8183=AXIS2_PLACEMENT_3D('',#12057,#9877,#9878);
#8184=AXIS2_PLACEMENT_3D('',#12058,#9879,#9880);
#8185=AXIS2_PLACEMENT_3D('',#12060,#9881,#9882);
#8186=AXIS2_PLACEMENT_3D('',#12063,#9884,#9885);
#8187=AXIS2_PLACEMENT_3D('',#12064,#9886,#9887);
#8188=AXIS2_PLACEMENT_3D('',#12066,#9888,#9889);
#8189=AXIS2_PLACEMENT_3D('',#12069,#9891,#9892);
#8190=AXIS2_PLACEMENT_3D('',#12070,#9893,#9894);
#8191=AXIS2_PLACEMENT_3D('',#12079,#9899,#9900);
#8192=AXIS2_PLACEMENT_3D('',#12085,#9904,#9905);
#8193=AXIS2_PLACEMENT_3D('',#12091,#9909,#9910);
#8194=AXIS2_PLACEMENT_3D('',#12097,#9914,#9915);
#8195=AXIS2_PLACEMENT_3D('',#12103,#9919,#9920);
#8196=AXIS2_PLACEMENT_3D('',#12106,#9923,#9924);
#8197=AXIS2_PLACEMENT_3D('',#12107,#9925,#9926);
#8198=AXIS2_PLACEMENT_3D('',#12108,#9927,#9928);
#8199=AXIS2_PLACEMENT_3D('',#12109,#9929,#9930);
#8200=AXIS2_PLACEMENT_3D('',#12110,#9931,#9932);
#8201=AXIS2_PLACEMENT_3D('',#12114,#9934,#9935);
#8202=AXIS2_PLACEMENT_3D('',#12115,#9936,#9937);
#8203=AXIS2_PLACEMENT_3D('',#12119,#9939,#9940);
#8204=AXIS2_PLACEMENT_3D('',#12122,#9942,#9943);
#8205=AXIS2_PLACEMENT_3D('',#12124,#9944,#9945);
#8206=AXIS2_PLACEMENT_3D('',#12126,#9947,#9948);
#8207=AXIS2_PLACEMENT_3D('',#12130,#9950,#9951);
#8208=AXIS2_PLACEMENT_3D('',#12131,#9952,#9953);
#8209=AXIS2_PLACEMENT_3D('',#12135,#9955,#9956);
#8210=AXIS2_PLACEMENT_3D('',#12138,#9958,#9959);
#8211=AXIS2_PLACEMENT_3D('',#12140,#9960,#9961);
#8212=AXIS2_PLACEMENT_3D('',#12142,#9963,#9964);
#8213=AXIS2_PLACEMENT_3D('',#12146,#9966,#9967);
#8214=AXIS2_PLACEMENT_3D('',#12147,#9968,#9969);
#8215=AXIS2_PLACEMENT_3D('',#12151,#9971,#9972);
#8216=AXIS2_PLACEMENT_3D('',#12154,#9974,#9975);
#8217=AXIS2_PLACEMENT_3D('',#12156,#9976,#9977);
#8218=AXIS2_PLACEMENT_3D('',#12158,#9979,#9980);
#8219=AXIS2_PLACEMENT_3D('',#12162,#9982,#9983);
#8220=AXIS2_PLACEMENT_3D('',#12163,#9984,#9985);
#8221=AXIS2_PLACEMENT_3D('',#12167,#9987,#9988);
#8222=AXIS2_PLACEMENT_3D('',#12170,#9990,#9991);
#8223=AXIS2_PLACEMENT_3D('',#12172,#9992,#9993);
#8224=AXIS2_PLACEMENT_3D('',#12174,#9995,#9996);
#8225=AXIS2_PLACEMENT_3D('',#12185,#10003,#10004);
#8226=AXIS2_PLACEMENT_3D('',#12196,#10011,#10012);
#8227=AXIS2_PLACEMENT_3D('',#12215,#10023,#10024);
#8228=AXIS2_PLACEMENT_3D('',#12219,#10027,#10028);
#8229=AXIS2_PLACEMENT_3D('',#12223,#10031,#10032);
#8230=AXIS2_PLACEMENT_3D('',#12227,#10035,#10036);
#8231=AXIS2_PLACEMENT_3D('',#12231,#10039,#10040);
#8232=AXIS2_PLACEMENT_3D('',#12233,#10042,#10043);
#8233=AXIS2_PLACEMENT_3D('',#12237,#10046,#10047);
#8234=AXIS2_PLACEMENT_3D('',#12241,#10050,#10051);
#8235=AXIS2_PLACEMENT_3D('',#12245,#10054,#10055);
#8236=AXIS2_PLACEMENT_3D('',#12249,#10058,#10059);
#8237=AXIS2_PLACEMENT_3D('',#12251,#10061,#10062);
#8238=AXIS2_PLACEMENT_3D('',#12252,#10063,#10064);
#8239=AXIS2_PLACEMENT_3D('',#12253,#10065,#10066);
#8240=AXIS2_PLACEMENT_3D('',#12262,#10071,#10072);
#8241=AXIS2_PLACEMENT_3D('',#12268,#10076,#10077);
#8242=AXIS2_PLACEMENT_3D('',#12274,#10081,#10082);
#8243=AXIS2_PLACEMENT_3D('',#12280,#10086,#10087);
#8244=AXIS2_PLACEMENT_3D('',#12286,#10091,#10092);
#8245=AXIS2_PLACEMENT_3D('',#12292,#10096,#10097);
#8246=AXIS2_PLACEMENT_3D('',#12298,#10101,#10102);
#8247=AXIS2_PLACEMENT_3D('',#12301,#10105,#10106);
#8248=AXIS2_PLACEMENT_3D('',#12302,#10107,#10108);
#8249=AXIS2_PLACEMENT_3D('',#12303,#10109,#10110);
#8250=AXIS2_PLACEMENT_3D('',#12304,#10111,#10112);
#8251=AXIS2_PLACEMENT_3D('',#12313,#10117,#10118);
#8252=AXIS2_PLACEMENT_3D('',#12319,#10122,#10123);
#8253=AXIS2_PLACEMENT_3D('',#12325,#10127,#10128);
#8254=AXIS2_PLACEMENT_3D('',#12331,#10132,#10133);
#8255=AXIS2_PLACEMENT_3D('',#12337,#10137,#10138);
#8256=AXIS2_PLACEMENT_3D('',#12343,#10142,#10143);
#8257=AXIS2_PLACEMENT_3D('',#12349,#10147,#10148);
#8258=AXIS2_PLACEMENT_3D('',#12352,#10151,#10152);
#8259=AXIS2_PLACEMENT_3D('',#12353,#10153,#10154);
#8260=AXIS2_PLACEMENT_3D('',#12354,#10155,#10156);
#8261=AXIS2_PLACEMENT_3D('',#12355,#10157,#10158);
#8262=AXIS2_PLACEMENT_3D('',#12356,#10159,#10160);
#8263=AXIS2_PLACEMENT_3D('',#12357,#10161,#10162);
#8264=AXIS2_PLACEMENT_3D('',#12358,#10163,#10164);
#8265=AXIS2_PLACEMENT_3D('',#12360,#10165,#10166);
#8266=AXIS2_PLACEMENT_3D('',#12363,#10168,#10169);
#8267=AXIS2_PLACEMENT_3D('',#12364,#10170,#10171);
#8268=AXIS2_PLACEMENT_3D('',#12367,#10173,#10174);
#8269=AXIS2_PLACEMENT_3D('',#12368,#10175,#10176);
#8270=AXIS2_PLACEMENT_3D('',#12370,#10177,#10178);
#8271=AXIS2_PLACEMENT_3D('',#12371,#10179,#10180);
#8272=AXIS2_PLACEMENT_3D('',#12374,#10182,#10183);
#8273=AXIS2_PLACEMENT_3D('',#12375,#10184,#10185);
#8274=AXIS2_PLACEMENT_3D('',#12376,#10186,#10187);
#8275=AXIS2_PLACEMENT_3D('',#12377,#10188,#10189);
#8276=AXIS2_PLACEMENT_3D('',#12378,#10190,#10191);
#8277=AXIS2_PLACEMENT_3D('',#12379,#10192,#10193);
#8278=AXIS2_PLACEMENT_3D('',#12380,#10194,#10195);
#8279=AXIS2_PLACEMENT_3D('',#12381,#10196,#10197);
#8280=AXIS2_PLACEMENT_3D('',#12382,#10198,#10199);
#8281=AXIS2_PLACEMENT_3D('',#12383,#10200,#10201);
#8282=AXIS2_PLACEMENT_3D('',#12384,#10202,#10203);
#8283=AXIS2_PLACEMENT_3D('',#12385,#10204,#10205);
#8284=AXIS2_PLACEMENT_3D('',#12386,#10206,#10207);
#8285=AXIS2_PLACEMENT_3D('',#12387,#10208,#10209);
#8286=AXIS2_PLACEMENT_3D('',#12388,#10210,#10211);
#8287=AXIS2_PLACEMENT_3D('',#12389,#10212,#10213);
#8288=AXIS2_PLACEMENT_3D('',#12390,#10214,#10215);
#8289=AXIS2_PLACEMENT_3D('',#12391,#10216,#10217);
#8290=AXIS2_PLACEMENT_3D('',#12392,#10218,#10219);
#8291=AXIS2_PLACEMENT_3D('',#12393,#10220,#10221);
#8292=AXIS2_PLACEMENT_3D('',#12394,#10222,#10223);
#8293=AXIS2_PLACEMENT_3D('',#12395,#10224,#10225);
#8294=AXIS2_PLACEMENT_3D('',#12396,#10226,#10227);
#8295=AXIS2_PLACEMENT_3D('',#12397,#10228,#10229);
#8296=AXIS2_PLACEMENT_3D('',#12398,#10230,#10231);
#8297=AXIS2_PLACEMENT_3D('',#12399,#10232,#10233);
#8298=AXIS2_PLACEMENT_3D('',#12400,#10234,#10235);
#8299=AXIS2_PLACEMENT_3D('',#12401,#10236,#10237);
#8300=AXIS2_PLACEMENT_3D('',#12402,#10238,#10239);
#8301=AXIS2_PLACEMENT_3D('',#12403,#10240,#10241);
#8302=AXIS2_PLACEMENT_3D('',#12404,#10242,#10243);
#8303=AXIS2_PLACEMENT_3D('',#12405,#10244,#10245);
#8304=AXIS2_PLACEMENT_3D('',#12406,#10246,#10247);
#8305=AXIS2_PLACEMENT_3D('',#12407,#10248,#10249);
#8306=AXIS2_PLACEMENT_3D('',#12408,#10250,#10251);
#8307=AXIS2_PLACEMENT_3D('',#12409,#10252,#10253);
#8308=AXIS2_PLACEMENT_3D('',#12410,#10254,#10255);
#8309=AXIS2_PLACEMENT_3D('',#12411,#10256,#10257);
#8310=AXIS2_PLACEMENT_3D('',#12412,#10258,#10259);
#8311=AXIS2_PLACEMENT_3D('',#12413,#10260,#10261);
#8312=AXIS2_PLACEMENT_3D('',#12414,#10262,#10263);
#8313=AXIS2_PLACEMENT_3D('',#12415,#10264,#10265);
#8314=AXIS2_PLACEMENT_3D('',#12416,#10266,#10267);
#8315=AXIS2_PLACEMENT_3D('',#12417,#10268,#10269);
#8316=AXIS2_PLACEMENT_3D('',#12418,#10270,#10271);
#8317=AXIS2_PLACEMENT_3D('',#12419,#10272,#10273);
#8318=AXIS2_PLACEMENT_3D('',#12420,#10274,#10275);
#8319=AXIS2_PLACEMENT_3D('',#12421,#10276,#10277);
#8320=AXIS2_PLACEMENT_3D('',#12422,#10278,#10279);
#8321=AXIS2_PLACEMENT_3D('',#12423,#10280,#10281);
#8322=AXIS2_PLACEMENT_3D('',#12424,#10282,#10283);
#8323=AXIS2_PLACEMENT_3D('',#12425,#10284,#10285);
#8324=AXIS2_PLACEMENT_3D('',#12426,#10286,#10287);
#8325=AXIS2_PLACEMENT_3D('',#12427,#10288,#10289);
#8326=AXIS2_PLACEMENT_3D('',#12428,#10290,#10291);
#8327=AXIS2_PLACEMENT_3D('',#12429,#10292,#10293);
#8328=AXIS2_PLACEMENT_3D('',#12430,#10294,#10295);
#8329=AXIS2_PLACEMENT_3D('',#12431,#10296,#10297);
#8330=AXIS2_PLACEMENT_3D('',#12432,#10298,#10299);
#8331=AXIS2_PLACEMENT_3D('',#12433,#10300,#10301);
#8332=AXIS2_PLACEMENT_3D('',#12434,#10302,#10303);
#8333=AXIS2_PLACEMENT_3D('',#12435,#10304,#10305);
#8334=AXIS2_PLACEMENT_3D('',#12436,#10306,#10307);
#8335=AXIS2_PLACEMENT_3D('',#12437,#10308,#10309);
#8336=AXIS2_PLACEMENT_3D('',#12438,#10310,#10311);
#8337=AXIS2_PLACEMENT_3D('',#12439,#10312,#10313);
#8338=AXIS2_PLACEMENT_3D('',#12440,#10314,#10315);
#8339=AXIS2_PLACEMENT_3D('',#12441,#10316,#10317);
#8340=AXIS2_PLACEMENT_3D('',#12442,#10318,#10319);
#8341=AXIS2_PLACEMENT_3D('',#12443,#10320,#10321);
#8342=AXIS2_PLACEMENT_3D('',#12444,#10322,#10323);
#8343=AXIS2_PLACEMENT_3D('',#12445,#10324,#10325);
#8344=AXIS2_PLACEMENT_3D('',#12446,#10326,#10327);
#8345=AXIS2_PLACEMENT_3D('',#12447,#10328,#10329);
#8346=AXIS2_PLACEMENT_3D('',#12449,#10330,#10331);
#8347=AXIS2_PLACEMENT_3D('',#12450,#10332,#10333);
#8348=AXIS2_PLACEMENT_3D('',#12452,#10334,#10335);
#8349=AXIS2_PLACEMENT_3D('',#12454,#10337,#10338);
#8350=AXIS2_PLACEMENT_3D('',#12456,#10339,#10340);
#8351=AXIS2_PLACEMENT_3D('',#12458,#10342,#10343);
#8352=AXIS2_PLACEMENT_3D('',#12460,#10344,#10345);
#8353=AXIS2_PLACEMENT_3D('',#12462,#10347,#10348);
#8354=AXIS2_PLACEMENT_3D('',#12464,#10349,#10350);
#8355=AXIS2_PLACEMENT_3D('',#12465,#10351,#10352);
#8356=AXIS2_PLACEMENT_3D('',#12467,#10353,#10354);
#8357=AXIS2_PLACEMENT_3D('',#12469,#10356,#10357);
#8358=AXIS2_PLACEMENT_3D('',#12471,#10358,#10359);
#8359=AXIS2_PLACEMENT_3D('',#12473,#10361,#10362);
#8360=AXIS2_PLACEMENT_3D('',#12475,#10363,#10364);
#8361=AXIS2_PLACEMENT_3D('',#12477,#10366,#10367);
#8362=AXIS2_PLACEMENT_3D('',#12478,#10368,#10369);
#8363=AXIS2_PLACEMENT_3D('',#12487,#10374,#10375);
#8364=AXIS2_PLACEMENT_3D('',#12493,#10379,#10380);
#8365=AXIS2_PLACEMENT_3D('',#12499,#10384,#10385);
#8366=AXIS2_PLACEMENT_3D('',#12505,#10389,#10390);
#8367=AXIS2_PLACEMENT_3D('',#12511,#10394,#10395);
#8368=AXIS2_PLACEMENT_3D('',#12514,#10398,#10399);
#8369=AXIS2_PLACEMENT_3D('',#12515,#10400,#10401);
#8370=AXIS2_PLACEMENT_3D('',#12516,#10402,#10403);
#8371=AXIS2_PLACEMENT_3D('',#12517,#10404,#10405);
#8372=AXIS2_PLACEMENT_3D('',#12519,#10406,#10407);
#8373=AXIS2_PLACEMENT_3D('',#12522,#10409,#10410);
#8374=AXIS2_PLACEMENT_3D('',#12523,#10411,#10412);
#8375=AXIS2_PLACEMENT_3D('',#12525,#10413,#10414);
#8376=AXIS2_PLACEMENT_3D('',#12528,#10416,#10417);
#8377=AXIS2_PLACEMENT_3D('',#12529,#10418,#10419);
#8378=AXIS2_PLACEMENT_3D('',#12530,#10420,#10421);
#8379=AXIS2_PLACEMENT_3D('',#12531,#10422,#10423);
#8380=AXIS2_PLACEMENT_3D('',#12532,#10424,#10425);
#8381=AXIS2_PLACEMENT_3D('',#12534,#10426,#10427);
#8382=AXIS2_PLACEMENT_3D('',#12535,#10428,#10429);
#8383=AXIS2_PLACEMENT_3D('',#12537,#10430,#10431);
#8384=AXIS2_PLACEMENT_3D('',#12539,#10433,#10434);
#8385=AXIS2_PLACEMENT_3D('',#12541,#10435,#10436);
#8386=AXIS2_PLACEMENT_3D('',#12543,#10438,#10439);
#8387=AXIS2_PLACEMENT_3D('',#12545,#10440,#10441);
#8388=AXIS2_PLACEMENT_3D('',#12547,#10443,#10444);
#8389=AXIS2_PLACEMENT_3D('',#12549,#10445,#10446);
#8390=AXIS2_PLACEMENT_3D('',#12550,#10447,#10448);
#8391=AXIS2_PLACEMENT_3D('',#12552,#10449,#10450);
#8392=AXIS2_PLACEMENT_3D('',#12554,#10452,#10453);
#8393=AXIS2_PLACEMENT_3D('',#12556,#10454,#10455);
#8394=AXIS2_PLACEMENT_3D('',#12558,#10457,#10458);
#8395=AXIS2_PLACEMENT_3D('',#12560,#10459,#10460);
#8396=AXIS2_PLACEMENT_3D('',#12562,#10462,#10463);
#8397=AXIS2_PLACEMENT_3D('',#12563,#10464,#10465);
#8398=AXIS2_PLACEMENT_3D('',#12572,#10470,#10471);
#8399=AXIS2_PLACEMENT_3D('',#12578,#10475,#10476);
#8400=AXIS2_PLACEMENT_3D('',#12584,#10480,#10481);
#8401=AXIS2_PLACEMENT_3D('',#12590,#10485,#10486);
#8402=AXIS2_PLACEMENT_3D('',#12596,#10490,#10491);
#8403=AXIS2_PLACEMENT_3D('',#12599,#10494,#10495);
#8404=AXIS2_PLACEMENT_3D('',#12600,#10496,#10497);
#8405=AXIS2_PLACEMENT_3D('',#12601,#10498,#10499);
#8406=AXIS2_PLACEMENT_3D('',#12602,#10500,#10501);
#8407=AXIS2_PLACEMENT_3D('',#12604,#10502,#10503);
#8408=AXIS2_PLACEMENT_3D('',#12607,#10505,#10506);
#8409=AXIS2_PLACEMENT_3D('',#12608,#10507,#10508);
#8410=AXIS2_PLACEMENT_3D('',#12611,#10510,#10511);
#8411=AXIS2_PLACEMENT_3D('',#12612,#10512,#10513);
#8412=AXIS2_PLACEMENT_3D('',#12614,#10514,#10515);
#8413=AXIS2_PLACEMENT_3D('',#12615,#10516,#10517);
#8414=AXIS2_PLACEMENT_3D('',#12618,#10519,#10520);
#8415=AXIS2_PLACEMENT_3D('',#12619,#10521,#10522);
#8416=AXIS2_PLACEMENT_3D('',#12620,#10523,#10524);
#8417=AXIS2_PLACEMENT_3D('',#12621,#10525,#10526);
#8418=AXIS2_PLACEMENT_3D('',#12630,#10531,#10532);
#8419=AXIS2_PLACEMENT_3D('',#12636,#10536,#10537);
#8420=AXIS2_PLACEMENT_3D('',#12642,#10541,#10542);
#8421=AXIS2_PLACEMENT_3D('',#12648,#10546,#10547);
#8422=AXIS2_PLACEMENT_3D('',#12654,#10551,#10552);
#8423=AXIS2_PLACEMENT_3D('',#12657,#10555,#10556);
#8424=AXIS2_PLACEMENT_3D('',#12658,#10557,#10558);
#8425=AXIS2_PLACEMENT_3D('',#12659,#10559,#10560);
#8426=AXIS2_PLACEMENT_3D('',#12661,#10561,#10562);
#8427=AXIS2_PLACEMENT_3D('',#12662,#10563,#10564);
#8428=AXIS2_PLACEMENT_3D('',#12664,#10565,#10566);
#8429=AXIS2_PLACEMENT_3D('',#12665,#10567,#10568);
#8430=AXIS2_PLACEMENT_3D('',#12667,#10569,#10570);
#8431=AXIS2_PLACEMENT_3D('',#12669,#10572,#10573);
#8432=AXIS2_PLACEMENT_3D('',#12671,#10574,#10575);
#8433=AXIS2_PLACEMENT_3D('',#12673,#10577,#10578);
#8434=AXIS2_PLACEMENT_3D('',#12675,#10579,#10580);
#8435=AXIS2_PLACEMENT_3D('',#12677,#10582,#10583);
#8436=AXIS2_PLACEMENT_3D('',#12679,#10584,#10585);
#8437=AXIS2_PLACEMENT_3D('',#12680,#10586,#10587);
#8438=AXIS2_PLACEMENT_3D('',#12682,#10588,#10589);
#8439=AXIS2_PLACEMENT_3D('',#12684,#10591,#10592);
#8440=AXIS2_PLACEMENT_3D('',#12686,#10594,#10595);
#8441=AXIS2_PLACEMENT_3D('',#12687,#10596,#10597);
#8442=AXIS2_PLACEMENT_3D('',#12688,#10598,#10599);
#8443=AXIS2_PLACEMENT_3D('',#12689,#10600,#10601);
#8444=AXIS2_PLACEMENT_3D('',#12690,#10602,#10603);
#8445=AXIS2_PLACEMENT_3D('',#12691,#10604,#10605);
#8446=AXIS2_PLACEMENT_3D('',#12692,#10606,#10607);
#8447=AXIS2_PLACEMENT_3D('',#12693,#10608,#10609);
#8448=AXIS2_PLACEMENT_3D('',#12694,#10610,#10611);
#8449=AXIS2_PLACEMENT_3D('',#12695,#10612,#10613);
#8450=AXIS2_PLACEMENT_3D('',#12696,#10614,#10615);
#8451=AXIS2_PLACEMENT_3D('',#12697,#10616,#10617);
#8452=AXIS2_PLACEMENT_3D('',#12698,#10618,#10619);
#8453=AXIS2_PLACEMENT_3D('',#12699,#10620,#10621);
#8454=AXIS2_PLACEMENT_3D('',#12700,#10622,#10623);
#8455=AXIS2_PLACEMENT_3D('',#12701,#10624,#10625);
#8456=AXIS2_PLACEMENT_3D('',#12702,#10626,#10627);
#8457=AXIS2_PLACEMENT_3D('',#12703,#10628,#10629);
#8458=AXIS2_PLACEMENT_3D('',#12704,#10630,#10631);
#8459=AXIS2_PLACEMENT_3D('',#12705,#10632,#10633);
#8460=AXIS2_PLACEMENT_3D('',#12706,#10634,#10635);
#8461=AXIS2_PLACEMENT_3D('',#12707,#10636,#10637);
#8462=AXIS2_PLACEMENT_3D('',#12708,#10638,#10639);
#8463=AXIS2_PLACEMENT_3D('',#12709,#10640,#10641);
#8464=AXIS2_PLACEMENT_3D('',#12710,#10642,#10643);
#8465=AXIS2_PLACEMENT_3D('',#12711,#10644,#10645);
#8466=AXIS2_PLACEMENT_3D('',#12712,#10646,#10647);
#8467=AXIS2_PLACEMENT_3D('',#12713,#10648,#10649);
#8468=AXIS2_PLACEMENT_3D('',#12714,#10650,#10651);
#8469=AXIS2_PLACEMENT_3D('',#12715,#10652,#10653);
#8470=AXIS2_PLACEMENT_3D('',#12716,#10654,#10655);
#8471=AXIS2_PLACEMENT_3D('',#12717,#10656,#10657);
#8472=AXIS2_PLACEMENT_3D('',#12718,#10658,#10659);
#8473=AXIS2_PLACEMENT_3D('',#12719,#10660,#10661);
#8474=AXIS2_PLACEMENT_3D('',#12720,#10662,#10663);
#8475=AXIS2_PLACEMENT_3D('',#12721,#10664,#10665);
#8476=AXIS2_PLACEMENT_3D('',#12722,#10666,#10667);
#8477=AXIS2_PLACEMENT_3D('',#12723,#10668,#10669);
#8478=AXIS2_PLACEMENT_3D('',#12724,#10670,#10671);
#8479=AXIS2_PLACEMENT_3D('',#12725,#10672,#10673);
#8480=AXIS2_PLACEMENT_3D('',#12726,#10674,#10675);
#8481=AXIS2_PLACEMENT_3D('',#12727,#10676,#10677);
#8482=AXIS2_PLACEMENT_3D('',#12728,#10678,#10679);
#8483=AXIS2_PLACEMENT_3D('',#12729,#10680,#10681);
#8484=AXIS2_PLACEMENT_3D('',#12730,#10682,#10683);
#8485=AXIS2_PLACEMENT_3D('',#12731,#10684,#10685);
#8486=AXIS2_PLACEMENT_3D('',#12732,#10686,#10687);
#8487=DIRECTION('axis',(0.,0.,1.));
#8488=DIRECTION('refdir',(1.,0.,0.));
#8489=DIRECTION('axis',(0.,0.,1.));
#8490=DIRECTION('refdir',(1.,0.,0.));
#8491=DIRECTION('axis',(0.,0.,1.));
#8492=DIRECTION('refdir',(1.,0.,0.));
#8493=DIRECTION('center_axis',(0.,0.,1.));
#8494=DIRECTION('ref_axis',(1.,0.,0.));
#8495=DIRECTION('center_axis',(0.,0.,1.));
#8496=DIRECTION('ref_axis',(1.,0.,0.));
#8497=DIRECTION('',(0.,0.,1.));
#8498=DIRECTION('center_axis',(0.,0.,-1.));
#8499=DIRECTION('ref_axis',(1.,0.,0.));
#8500=DIRECTION('center_axis',(0.,0.,1.));
#8501=DIRECTION('ref_axis',(1.,0.,0.));
#8502=DIRECTION('center_axis',(0.,0.,1.));
#8503=DIRECTION('ref_axis',(1.,0.,0.));
#8504=DIRECTION('',(0.,0.,1.));
#8505=DIRECTION('center_axis',(0.,0.,-1.));
#8506=DIRECTION('ref_axis',(1.,0.,0.));
#8507=DIRECTION('center_axis',(0.,0.,1.));
#8508=DIRECTION('ref_axis',(1.,0.,0.));
#8509=DIRECTION('center_axis',(0.,0.,1.));
#8510=DIRECTION('ref_axis',(1.,0.,0.));
#8511=DIRECTION('',(0.,0.,1.));
#8512=DIRECTION('center_axis',(0.,0.,-1.));
#8513=DIRECTION('ref_axis',(1.,0.,0.));
#8514=DIRECTION('center_axis',(0.,0.,1.));
#8515=DIRECTION('ref_axis',(1.,0.,0.));
#8516=DIRECTION('center_axis',(0.,0.,1.));
#8517=DIRECTION('ref_axis',(1.,0.,0.));
#8518=DIRECTION('',(0.,0.,1.));
#8519=DIRECTION('center_axis',(0.,0.,-1.));
#8520=DIRECTION('ref_axis',(1.,0.,0.));
#8521=DIRECTION('center_axis',(0.,0.,1.));
#8522=DIRECTION('ref_axis',(1.,0.,0.));
#8523=DIRECTION('center_axis',(0.,0.,1.));
#8524=DIRECTION('ref_axis',(1.,0.,0.));
#8525=DIRECTION('',(0.,0.,1.));
#8526=DIRECTION('center_axis',(0.,0.,-1.));
#8527=DIRECTION('ref_axis',(1.,0.,0.));
#8528=DIRECTION('center_axis',(0.,0.,1.));
#8529=DIRECTION('ref_axis',(1.,0.,0.));
#8530=DIRECTION('center_axis',(0.,0.,1.));
#8531=DIRECTION('ref_axis',(1.,0.,0.));
#8532=DIRECTION('',(0.,0.,1.));
#8533=DIRECTION('center_axis',(0.,0.,-1.));
#8534=DIRECTION('ref_axis',(1.,0.,0.));
#8535=DIRECTION('center_axis',(0.,1.,0.));
#8536=DIRECTION('ref_axis',(-1.,0.,0.));
#8537=DIRECTION('',(-1.,0.,0.));
#8538=DIRECTION('',(0.,0.,1.));
#8539=DIRECTION('',(-1.,0.,0.));
#8540=DIRECTION('',(0.,0.,1.));
#8541=DIRECTION('center_axis',(1.,0.,0.));
#8542=DIRECTION('ref_axis',(0.,1.,0.));
#8543=DIRECTION('',(0.,1.,0.));
#8544=DIRECTION('',(0.,1.,0.));
#8545=DIRECTION('',(0.,0.,1.));
#8546=DIRECTION('center_axis',(0.,-1.,0.));
#8547=DIRECTION('ref_axis',(1.,0.,0.));
#8548=DIRECTION('',(1.,0.,0.));
#8549=DIRECTION('',(1.,0.,0.));
#8550=DIRECTION('',(0.,0.,1.));
#8551=DIRECTION('center_axis',(-1.,0.,0.));
#8552=DIRECTION('ref_axis',(0.,-1.,0.));
#8553=DIRECTION('',(0.,-1.,0.));
#8554=DIRECTION('',(0.,-1.,0.));
#8555=DIRECTION('center_axis',(0.,0.,1.));
#8556=DIRECTION('ref_axis',(1.,0.,0.));
#8557=DIRECTION('center_axis',(0.,0.,1.));
#8558=DIRECTION('ref_axis',(1.,0.,0.));
#8559=DIRECTION('axis',(0.,0.,1.));
#8560=DIRECTION('refdir',(1.,0.,0.));
#8561=DIRECTION('center_axis',(0.,0.,1.));
#8562=DIRECTION('ref_axis',(1.,0.,0.));
#8563=DIRECTION('center_axis',(0.,0.,1.));
#8564=DIRECTION('ref_axis',(1.,0.,0.));
#8565=DIRECTION('',(0.,0.,1.));
#8566=DIRECTION('center_axis',(0.,0.,-1.));
#8567=DIRECTION('ref_axis',(1.,0.,0.));
#8568=DIRECTION('center_axis',(0.,0.,1.));
#8569=DIRECTION('ref_axis',(1.,0.,0.));
#8570=DIRECTION('center_axis',(0.,0.,1.));
#8571=DIRECTION('ref_axis',(1.,0.,0.));
#8572=DIRECTION('',(0.,0.,1.));
#8573=DIRECTION('center_axis',(0.,0.,-1.));
#8574=DIRECTION('ref_axis',(1.,0.,0.));
#8575=DIRECTION('center_axis',(0.,0.,1.));
#8576=DIRECTION('ref_axis',(1.,0.,0.));
#8577=DIRECTION('center_axis',(0.,0.,1.));
#8578=DIRECTION('ref_axis',(1.,0.,0.));
#8579=DIRECTION('',(0.,0.,1.));
#8580=DIRECTION('center_axis',(0.,0.,-1.));
#8581=DIRECTION('ref_axis',(1.,0.,0.));
#8582=DIRECTION('center_axis',(0.,0.,1.));
#8583=DIRECTION('ref_axis',(1.,0.,0.));
#8584=DIRECTION('center_axis',(0.,0.,1.));
#8585=DIRECTION('ref_axis',(1.,0.,0.));
#8586=DIRECTION('',(0.,0.,1.));
#8587=DIRECTION('center_axis',(0.,0.,-1.));
#8588=DIRECTION('ref_axis',(1.,0.,0.));
#8589=DIRECTION('center_axis',(0.,0.,1.));
#8590=DIRECTION('ref_axis',(1.,0.,0.));
#8591=DIRECTION('center_axis',(0.,0.,1.));
#8592=DIRECTION('ref_axis',(1.,0.,0.));
#8593=DIRECTION('',(0.,0.,1.));
#8594=DIRECTION('center_axis',(0.,0.,-1.));
#8595=DIRECTION('ref_axis',(1.,0.,0.));
#8596=DIRECTION('center_axis',(0.,0.,1.));
#8597=DIRECTION('ref_axis',(1.,0.,0.));
#8598=DIRECTION('center_axis',(0.,0.,1.));
#8599=DIRECTION('ref_axis',(1.,0.,0.));
#8600=DIRECTION('',(0.,0.,1.));
#8601=DIRECTION('center_axis',(0.,0.,-1.));
#8602=DIRECTION('ref_axis',(1.,0.,0.));
#8603=DIRECTION('center_axis',(0.,1.,0.));
#8604=DIRECTION('ref_axis',(-1.,0.,0.));
#8605=DIRECTION('',(-1.,0.,0.));
#8606=DIRECTION('',(0.,0.,1.));
#8607=DIRECTION('',(-1.,0.,0.));
#8608=DIRECTION('',(0.,0.,1.));
#8609=DIRECTION('center_axis',(1.,0.,0.));
#8610=DIRECTION('ref_axis',(0.,1.,0.));
#8611=DIRECTION('',(0.,1.,0.));
#8612=DIRECTION('',(0.,1.,0.));
#8613=DIRECTION('',(0.,0.,1.));
#8614=DIRECTION('center_axis',(0.,-1.,0.));
#8615=DIRECTION('ref_axis',(1.,0.,0.));
#8616=DIRECTION('',(1.,0.,0.));
#8617=DIRECTION('',(1.,0.,0.));
#8618=DIRECTION('',(0.,0.,1.));
#8619=DIRECTION('center_axis',(-1.,0.,0.));
#8620=DIRECTION('ref_axis',(0.,-1.,0.));
#8621=DIRECTION('',(0.,-1.,0.));
#8622=DIRECTION('',(0.,-1.,0.));
#8623=DIRECTION('center_axis',(0.,0.,1.));
#8624=DIRECTION('ref_axis',(1.,0.,0.));
#8625=DIRECTION('center_axis',(0.,0.,1.));
#8626=DIRECTION('ref_axis',(1.,0.,0.));
#8627=DIRECTION('axis',(0.,0.,1.));
#8628=DIRECTION('refdir',(1.,0.,0.));
#8629=DIRECTION('center_axis',(0.,0.,1.));
#8630=DIRECTION('ref_axis',(1.,0.,0.));
#8631=DIRECTION('center_axis',(0.,0.,1.));
#8632=DIRECTION('ref_axis',(1.,0.,0.));
#8633=DIRECTION('',(0.,0.,1.));
#8634=DIRECTION('center_axis',(0.,0.,-1.));
#8635=DIRECTION('ref_axis',(1.,0.,0.));
#8636=DIRECTION('center_axis',(0.,0.,1.));
#8637=DIRECTION('ref_axis',(1.,0.,0.));
#8638=DIRECTION('center_axis',(0.,0.,1.));
#8639=DIRECTION('ref_axis',(1.,0.,0.));
#8640=DIRECTION('',(0.,0.,1.));
#8641=DIRECTION('center_axis',(0.,0.,-1.));
#8642=DIRECTION('ref_axis',(1.,0.,0.));
#8643=DIRECTION('center_axis',(0.,1.,0.));
#8644=DIRECTION('ref_axis',(-1.,0.,0.));
#8645=DIRECTION('',(-1.,0.,0.));
#8646=DIRECTION('',(0.,0.,1.));
#8647=DIRECTION('',(-1.,0.,0.));
#8648=DIRECTION('',(0.,0.,1.));
#8649=DIRECTION('center_axis',(1.,0.,0.));
#8650=DIRECTION('ref_axis',(0.,1.,0.));
#8651=DIRECTION('',(0.,1.,0.));
#8652=DIRECTION('',(0.,1.,0.));
#8653=DIRECTION('',(0.,0.,1.));
#8654=DIRECTION('center_axis',(0.,-1.,0.));
#8655=DIRECTION('ref_axis',(1.,0.,0.));
#8656=DIRECTION('',(1.,0.,0.));
#8657=DIRECTION('',(1.,0.,0.));
#8658=DIRECTION('',(0.,0.,1.));
#8659=DIRECTION('center_axis',(-1.,0.,0.));
#8660=DIRECTION('ref_axis',(0.,-1.,0.));
#8661=DIRECTION('',(0.,-1.,0.));
#8662=DIRECTION('',(0.,-1.,0.));
#8663=DIRECTION('center_axis',(0.,0.,1.));
#8664=DIRECTION('ref_axis',(1.,0.,0.));
#8665=DIRECTION('center_axis',(0.,0.,1.));
#8666=DIRECTION('ref_axis',(1.,0.,0.));
#8667=DIRECTION('axis',(0.,0.,1.));
#8668=DIRECTION('refdir',(1.,0.,0.));
#8669=DIRECTION('center_axis',(0.,0.,1.));
#8670=DIRECTION('ref_axis',(1.,0.,0.));
#8671=DIRECTION('center_axis',(0.,0.,1.));
#8672=DIRECTION('ref_axis',(1.,0.,0.));
#8673=DIRECTION('',(0.,0.,1.));
#8674=DIRECTION('center_axis',(0.,0.,-1.));
#8675=DIRECTION('ref_axis',(1.,0.,0.));
#8676=DIRECTION('center_axis',(0.,0.,1.));
#8677=DIRECTION('ref_axis',(1.,0.,0.));
#8678=DIRECTION('center_axis',(0.,0.,1.));
#8679=DIRECTION('ref_axis',(1.,0.,0.));
#8680=DIRECTION('',(0.,0.,1.));
#8681=DIRECTION('center_axis',(0.,0.,-1.));
#8682=DIRECTION('ref_axis',(1.,0.,0.));
#8683=DIRECTION('center_axis',(0.,1.,0.));
#8684=DIRECTION('ref_axis',(-1.,0.,0.));
#8685=DIRECTION('',(-1.,0.,0.));
#8686=DIRECTION('',(0.,0.,1.));
#8687=DIRECTION('',(-1.,0.,0.));
#8688=DIRECTION('',(0.,0.,1.));
#8689=DIRECTION('center_axis',(1.,0.,0.));
#8690=DIRECTION('ref_axis',(0.,1.,0.));
#8691=DIRECTION('',(0.,1.,0.));
#8692=DIRECTION('',(0.,1.,0.));
#8693=DIRECTION('',(0.,0.,1.));
#8694=DIRECTION('center_axis',(0.,-1.,0.));
#8695=DIRECTION('ref_axis',(1.,0.,0.));
#8696=DIRECTION('',(1.,0.,0.));
#8697=DIRECTION('',(1.,0.,0.));
#8698=DIRECTION('',(0.,0.,1.));
#8699=DIRECTION('center_axis',(-1.,0.,0.));
#8700=DIRECTION('ref_axis',(0.,-1.,0.));
#8701=DIRECTION('',(0.,-1.,0.));
#8702=DIRECTION('',(0.,-1.,0.));
#8703=DIRECTION('center_axis',(0.,0.,1.));
#8704=DIRECTION('ref_axis',(1.,0.,0.));
#8705=DIRECTION('center_axis',(0.,0.,1.));
#8706=DIRECTION('ref_axis',(1.,0.,0.));
#8707=DIRECTION('axis',(0.,0.,1.));
#8708=DIRECTION('refdir',(1.,0.,0.));
#8709=DIRECTION('center_axis',(0.,1.,0.));
#8710=DIRECTION('ref_axis',(-1.,0.,0.));
#8711=DIRECTION('',(-1.,0.,0.));
#8712=DIRECTION('',(0.,0.,1.));
#8713=DIRECTION('',(-1.,0.,0.));
#8714=DIRECTION('',(0.,0.,1.));
#8715=DIRECTION('center_axis',(1.,0.,0.));
#8716=DIRECTION('ref_axis',(0.,1.,0.));
#8717=DIRECTION('',(0.,1.,0.));
#8718=DIRECTION('',(0.,1.,0.));
#8719=DIRECTION('',(0.,0.,1.));
#8720=DIRECTION('center_axis',(0.,-1.,0.));
#8721=DIRECTION('ref_axis',(1.,0.,0.));
#8722=DIRECTION('',(1.,0.,0.));
#8723=DIRECTION('',(1.,0.,0.));
#8724=DIRECTION('',(0.,0.,1.));
#8725=DIRECTION('center_axis',(-1.,0.,0.));
#8726=DIRECTION('ref_axis',(0.,-1.,0.));
#8727=DIRECTION('',(0.,-1.,0.));
#8728=DIRECTION('',(0.,-1.,0.));
#8729=DIRECTION('center_axis',(0.,0.,1.));
#8730=DIRECTION('ref_axis',(1.,0.,0.));
#8731=DIRECTION('center_axis',(0.,0.,1.));
#8732=DIRECTION('ref_axis',(1.,0.,0.));
#8733=DIRECTION('axis',(0.,0.,1.));
#8734=DIRECTION('refdir',(1.,0.,0.));
#8735=DIRECTION('center_axis',(0.,1.,0.));
#8736=DIRECTION('ref_axis',(-1.,0.,0.));
#8737=DIRECTION('',(-1.,0.,0.));
#8738=DIRECTION('',(0.,0.,1.));
#8739=DIRECTION('',(-1.,0.,0.));
#8740=DIRECTION('',(0.,0.,1.));
#8741=DIRECTION('center_axis',(1.,0.,0.));
#8742=DIRECTION('ref_axis',(0.,1.,0.));
#8743=DIRECTION('',(0.,1.,0.));
#8744=DIRECTION('',(0.,1.,0.));
#8745=DIRECTION('',(0.,0.,1.));
#8746=DIRECTION('center_axis',(0.,-1.,0.));
#8747=DIRECTION('ref_axis',(1.,0.,0.));
#8748=DIRECTION('',(1.,0.,0.));
#8749=DIRECTION('',(1.,0.,0.));
#8750=DIRECTION('',(0.,0.,1.));
#8751=DIRECTION('center_axis',(-1.,0.,0.));
#8752=DIRECTION('ref_axis',(0.,-1.,0.));
#8753=DIRECTION('',(0.,-1.,0.));
#8754=DIRECTION('',(0.,-1.,0.));
#8755=DIRECTION('center_axis',(0.,0.,1.));
#8756=DIRECTION('ref_axis',(1.,0.,0.));
#8757=DIRECTION('center_axis',(0.,0.,1.));
#8758=DIRECTION('ref_axis',(1.,0.,0.));
#8759=DIRECTION('axis',(0.,0.,1.));
#8760=DIRECTION('refdir',(1.,0.,0.));
#8761=DIRECTION('center_axis',(0.,0.,1.));
#8762=DIRECTION('ref_axis',(1.,0.,0.));
#8763=DIRECTION('center_axis',(0.,0.,1.));
#8764=DIRECTION('ref_axis',(1.,0.,0.));
#8765=DIRECTION('',(0.,0.,1.));
#8766=DIRECTION('center_axis',(0.,0.,-1.));
#8767=DIRECTION('ref_axis',(1.,0.,0.));
#8768=DIRECTION('center_axis',(0.,0.,1.));
#8769=DIRECTION('ref_axis',(1.,0.,0.));
#8770=DIRECTION('center_axis',(0.,0.,1.));
#8771=DIRECTION('ref_axis',(1.,0.,0.));
#8772=DIRECTION('',(0.,0.,1.));
#8773=DIRECTION('center_axis',(0.,0.,-1.));
#8774=DIRECTION('ref_axis',(1.,0.,0.));
#8775=DIRECTION('center_axis',(0.,1.,0.));
#8776=DIRECTION('ref_axis',(-1.,0.,0.));
#8777=DIRECTION('',(-1.,0.,0.));
#8778=DIRECTION('',(0.,0.,1.));
#8779=DIRECTION('',(-1.,0.,0.));
#8780=DIRECTION('',(0.,0.,1.));
#8781=DIRECTION('center_axis',(1.,0.,0.));
#8782=DIRECTION('ref_axis',(0.,1.,0.));
#8783=DIRECTION('',(0.,1.,0.));
#8784=DIRECTION('',(0.,1.,0.));
#8785=DIRECTION('',(0.,0.,1.));
#8786=DIRECTION('center_axis',(0.,-1.,0.));
#8787=DIRECTION('ref_axis',(1.,0.,0.));
#8788=DIRECTION('',(1.,0.,0.));
#8789=DIRECTION('',(1.,0.,0.));
#8790=DIRECTION('',(0.,0.,1.));
#8791=DIRECTION('center_axis',(-1.,0.,0.));
#8792=DIRECTION('ref_axis',(0.,-1.,0.));
#8793=DIRECTION('',(0.,-1.,0.));
#8794=DIRECTION('',(0.,-1.,0.));
#8795=DIRECTION('center_axis',(0.,0.,1.));
#8796=DIRECTION('ref_axis',(1.,0.,0.));
#8797=DIRECTION('center_axis',(0.,0.,1.));
#8798=DIRECTION('ref_axis',(1.,0.,0.));
#8799=DIRECTION('axis',(0.,0.,1.));
#8800=DIRECTION('refdir',(1.,0.,0.));
#8801=DIRECTION('center_axis',(0.,0.,1.));
#8802=DIRECTION('ref_axis',(1.,0.,0.));
#8803=DIRECTION('center_axis',(0.,0.,1.));
#8804=DIRECTION('ref_axis',(1.,0.,0.));
#8805=DIRECTION('',(0.,0.,1.));
#8806=DIRECTION('center_axis',(0.,0.,-1.));
#8807=DIRECTION('ref_axis',(1.,0.,0.));
#8808=DIRECTION('center_axis',(0.,0.,1.));
#8809=DIRECTION('ref_axis',(1.,0.,0.));
#8810=DIRECTION('center_axis',(0.,0.,1.));
#8811=DIRECTION('ref_axis',(1.,0.,0.));
#8812=DIRECTION('',(0.,0.,1.));
#8813=DIRECTION('center_axis',(0.,0.,-1.));
#8814=DIRECTION('ref_axis',(1.,0.,0.));
#8815=DIRECTION('center_axis',(0.,1.,0.));
#8816=DIRECTION('ref_axis',(-1.,0.,0.));
#8817=DIRECTION('',(-1.,0.,0.));
#8818=DIRECTION('',(0.,0.,1.));
#8819=DIRECTION('',(-1.,0.,0.));
#8820=DIRECTION('',(0.,0.,1.));
#8821=DIRECTION('center_axis',(1.,0.,0.));
#8822=DIRECTION('ref_axis',(0.,1.,0.));
#8823=DIRECTION('',(0.,1.,0.));
#8824=DIRECTION('',(0.,1.,0.));
#8825=DIRECTION('',(0.,0.,1.));
#8826=DIRECTION('center_axis',(0.,-1.,0.));
#8827=DIRECTION('ref_axis',(1.,0.,0.));
#8828=DIRECTION('',(1.,0.,0.));
#8829=DIRECTION('',(1.,0.,0.));
#8830=DIRECTION('',(0.,0.,1.));
#8831=DIRECTION('center_axis',(-1.,0.,0.));
#8832=DIRECTION('ref_axis',(0.,-1.,0.));
#8833=DIRECTION('',(0.,-1.,0.));
#8834=DIRECTION('',(0.,-1.,0.));
#8835=DIRECTION('center_axis',(0.,0.,1.));
#8836=DIRECTION('ref_axis',(1.,0.,0.));
#8837=DIRECTION('center_axis',(0.,0.,1.));
#8838=DIRECTION('ref_axis',(1.,0.,0.));
#8839=DIRECTION('axis',(0.,0.,1.));
#8840=DIRECTION('refdir',(1.,0.,0.));
#8841=DIRECTION('center_axis',(0.,1.,0.));
#8842=DIRECTION('ref_axis',(-1.,0.,0.));
#8843=DIRECTION('',(-1.,0.,0.));
#8844=DIRECTION('',(0.,0.,1.));
#8845=DIRECTION('',(-1.,0.,0.));
#8846=DIRECTION('',(0.,0.,1.));
#8847=DIRECTION('center_axis',(1.,0.,0.));
#8848=DIRECTION('ref_axis',(0.,1.,0.));
#8849=DIRECTION('',(0.,1.,0.));
#8850=DIRECTION('',(0.,1.,0.));
#8851=DIRECTION('',(0.,0.,1.));
#8852=DIRECTION('center_axis',(0.,-1.,0.));
#8853=DIRECTION('ref_axis',(1.,0.,0.));
#8854=DIRECTION('',(1.,0.,0.));
#8855=DIRECTION('',(1.,0.,0.));
#8856=DIRECTION('',(0.,0.,1.));
#8857=DIRECTION('center_axis',(-1.,0.,0.));
#8858=DIRECTION('ref_axis',(0.,-1.,0.));
#8859=DIRECTION('',(0.,-1.,0.));
#8860=DIRECTION('',(0.,-1.,0.));
#8861=DIRECTION('center_axis',(0.,0.,1.));
#8862=DIRECTION('ref_axis',(1.,0.,0.));
#8863=DIRECTION('center_axis',(0.,0.,1.));
#8864=DIRECTION('ref_axis',(1.,0.,0.));
#8865=DIRECTION('axis',(0.,0.,1.));
#8866=DIRECTION('refdir',(1.,0.,0.));
#8867=DIRECTION('center_axis',(0.,1.,0.));
#8868=DIRECTION('ref_axis',(-1.,0.,0.));
#8869=DIRECTION('',(-1.,0.,0.));
#8870=DIRECTION('',(0.,0.,1.));
#8871=DIRECTION('',(-1.,0.,0.));
#8872=DIRECTION('',(0.,0.,1.));
#8873=DIRECTION('center_axis',(1.,0.,0.));
#8874=DIRECTION('ref_axis',(0.,1.,0.));
#8875=DIRECTION('',(0.,1.,0.));
#8876=DIRECTION('',(0.,1.,0.));
#8877=DIRECTION('',(0.,0.,1.));
#8878=DIRECTION('center_axis',(0.,-1.,0.));
#8879=DIRECTION('ref_axis',(1.,0.,0.));
#8880=DIRECTION('',(1.,0.,0.));
#8881=DIRECTION('',(1.,0.,0.));
#8882=DIRECTION('',(0.,0.,1.));
#8883=DIRECTION('center_axis',(-1.,0.,0.));
#8884=DIRECTION('ref_axis',(0.,-1.,0.));
#8885=DIRECTION('',(0.,-1.,0.));
#8886=DIRECTION('',(0.,-1.,0.));
#8887=DIRECTION('center_axis',(0.,0.,1.));
#8888=DIRECTION('ref_axis',(1.,0.,0.));
#8889=DIRECTION('center_axis',(0.,0.,1.));
#8890=DIRECTION('ref_axis',(1.,0.,0.));
#8891=DIRECTION('axis',(0.,0.,1.));
#8892=DIRECTION('refdir',(1.,0.,0.));
#8893=DIRECTION('center_axis',(0.,0.,1.));
#8894=DIRECTION('ref_axis',(1.,0.,0.));
#8895=DIRECTION('',(0.,0.,1.));
#8896=DIRECTION('center_axis',(0.,0.,-1.));
#8897=DIRECTION('ref_axis',(1.,0.,0.));
#8898=DIRECTION('',(0.,0.,1.));
#8899=DIRECTION('center_axis',(0.,0.,1.));
#8900=DIRECTION('ref_axis',(1.,0.,0.));
#8901=DIRECTION('center_axis',(0.,0.,1.));
#8902=DIRECTION('ref_axis',(1.,0.,0.));
#8903=DIRECTION('',(0.,0.,1.));
#8904=DIRECTION('center_axis',(0.,0.,1.));
#8905=DIRECTION('ref_axis',(1.,0.,0.));
#8906=DIRECTION('',(0.,0.,1.));
#8907=DIRECTION('center_axis',(0.,0.,-1.));
#8908=DIRECTION('ref_axis',(1.,0.,0.));
#8909=DIRECTION('center_axis',(0.,0.,1.));
#8910=DIRECTION('ref_axis',(1.,0.,0.));
#8911=DIRECTION('center_axis',(0.,0.,1.));
#8912=DIRECTION('ref_axis',(1.,0.,0.));
#8913=DIRECTION('center_axis',(0.,0.,1.));
#8914=DIRECTION('ref_axis',(1.,0.,0.));
#8915=DIRECTION('',(0.,0.,1.));
#8916=DIRECTION('center_axis',(0.,0.,-1.));
#8917=DIRECTION('ref_axis',(1.,0.,0.));
#8918=DIRECTION('',(0.,0.,1.));
#8919=DIRECTION('center_axis',(0.,0.,1.));
#8920=DIRECTION('ref_axis',(1.,0.,0.));
#8921=DIRECTION('center_axis',(0.,0.,1.));
#8922=DIRECTION('ref_axis',(1.,0.,0.));
#8923=DIRECTION('',(0.,0.,1.));
#8924=DIRECTION('center_axis',(0.,0.,1.));
#8925=DIRECTION('ref_axis',(1.,0.,0.));
#8926=DIRECTION('',(0.,0.,1.));
#8927=DIRECTION('center_axis',(0.,0.,-1.));
#8928=DIRECTION('ref_axis',(1.,0.,0.));
#8929=DIRECTION('center_axis',(0.,0.,1.));
#8930=DIRECTION('ref_axis',(1.,0.,0.));
#8931=DIRECTION('center_axis',(0.,0.,1.));
#8932=DIRECTION('ref_axis',(1.,0.,0.));
#8933=DIRECTION('center_axis',(0.,0.,1.));
#8934=DIRECTION('ref_axis',(1.,0.,0.));
#8935=DIRECTION('',(0.,1.,0.));
#8936=DIRECTION('',(-1.,0.,0.));
#8937=DIRECTION('',(0.,-1.,0.));
#8938=DIRECTION('center_axis',(0.,0.,1.));
#8939=DIRECTION('ref_axis',(1.,0.,0.));
#8940=DIRECTION('',(0.,1.,0.));
#8941=DIRECTION('',(0.,-1.,0.));
#8942=DIRECTION('center_axis',(0.,0.,1.));
#8943=DIRECTION('ref_axis',(1.,0.,0.));
#8944=DIRECTION('',(0.,-1.,0.));
#8945=DIRECTION('',(1.,0.,0.));
#8946=DIRECTION('',(0.,1.,0.));
#8947=DIRECTION('center_axis',(0.,0.,1.));
#8948=DIRECTION('ref_axis',(1.,0.,0.));
#8949=DIRECTION('center_axis',(0.,0.,1.));
#8950=DIRECTION('ref_axis',(1.,0.,0.));
#8951=DIRECTION('',(0.,0.,1.));
#8952=DIRECTION('center_axis',(0.,0.,1.));
#8953=DIRECTION('ref_axis',(1.,0.,0.));
#8954=DIRECTION('center_axis',(0.,0.,1.));
#8955=DIRECTION('ref_axis',(1.,0.,0.));
#8956=DIRECTION('',(0.,0.,1.));
#8957=DIRECTION('center_axis',(0.,1.,0.));
#8958=DIRECTION('ref_axis',(-1.,0.,0.));
#8959=DIRECTION('',(-1.,0.,0.));
#8960=DIRECTION('',(0.,0.,1.));
#8961=DIRECTION('',(0.,0.,1.));
#8962=DIRECTION('center_axis',(1.,0.,0.));
#8963=DIRECTION('ref_axis',(0.,1.,0.));
#8964=DIRECTION('',(0.,1.,0.));
#8965=DIRECTION('',(0.,0.,1.));
#8966=DIRECTION('center_axis',(0.,-1.,0.));
#8967=DIRECTION('ref_axis',(1.,0.,0.));
#8968=DIRECTION('',(1.,0.,0.));
#8969=DIRECTION('',(0.,0.,1.));
#8970=DIRECTION('center_axis',(-1.,0.,0.));
#8971=DIRECTION('ref_axis',(0.,-1.,0.));
#8972=DIRECTION('',(0.,-1.,0.));
#8973=DIRECTION('center_axis',(0.,0.,1.));
#8974=DIRECTION('ref_axis',(1.,0.,0.));
#8975=DIRECTION('axis',(0.,0.,1.));
#8976=DIRECTION('refdir',(1.,0.,0.));
#8977=DIRECTION('center_axis',(0.,1.,0.));
#8978=DIRECTION('ref_axis',(-1.,0.,0.));
#8979=DIRECTION('',(-1.,0.,0.));
#8980=DIRECTION('',(0.,0.,1.));
#8981=DIRECTION('',(-1.,0.,0.));
#8982=DIRECTION('',(0.,0.,1.));
#8983=DIRECTION('center_axis',(1.,0.,0.));
#8984=DIRECTION('ref_axis',(0.,1.,0.));
#8985=DIRECTION('',(0.,1.,0.));
#8986=DIRECTION('',(0.,1.,0.));
#8987=DIRECTION('',(0.,0.,1.));
#8988=DIRECTION('center_axis',(0.,-1.,0.));
#8989=DIRECTION('ref_axis',(1.,0.,0.));
#8990=DIRECTION('',(1.,0.,0.));
#8991=DIRECTION('',(1.,0.,0.));
#8992=DIRECTION('',(0.,0.,1.));
#8993=DIRECTION('center_axis',(-1.,0.,0.));
#8994=DIRECTION('ref_axis',(0.,-1.,0.));
#8995=DIRECTION('',(0.,-1.,0.));
#8996=DIRECTION('',(0.,-1.,0.));
#8997=DIRECTION('center_axis',(0.,0.,1.));
#8998=DIRECTION('ref_axis',(1.,0.,0.));
#8999=DIRECTION('center_axis',(0.,0.,1.));
#9000=DIRECTION('ref_axis',(1.,0.,0.));
#9001=DIRECTION('axis',(0.,0.,1.));
#9002=DIRECTION('refdir',(1.,0.,0.));
#9003=DIRECTION('center_axis',(0.,0.,1.));
#9004=DIRECTION('ref_axis',(1.,0.,0.));
#9005=DIRECTION('',(0.,0.,1.));
#9006=DIRECTION('center_axis',(0.,0.,-1.));
#9007=DIRECTION('ref_axis',(1.,0.,0.));
#9008=DIRECTION('',(0.,0.,1.));
#9009=DIRECTION('center_axis',(0.,0.,1.));
#9010=DIRECTION('ref_axis',(1.,0.,0.));
#9011=DIRECTION('center_axis',(0.,0.,1.));
#9012=DIRECTION('ref_axis',(1.,0.,0.));
#9013=DIRECTION('',(0.,0.,1.));
#9014=DIRECTION('center_axis',(0.,0.,1.));
#9015=DIRECTION('ref_axis',(1.,0.,0.));
#9016=DIRECTION('',(0.,0.,1.));
#9017=DIRECTION('center_axis',(0.,0.,-1.));
#9018=DIRECTION('ref_axis',(1.,0.,0.));
#9019=DIRECTION('center_axis',(0.,0.,1.));
#9020=DIRECTION('ref_axis',(1.,0.,0.));
#9021=DIRECTION('center_axis',(0.,0.,1.));
#9022=DIRECTION('ref_axis',(1.,0.,0.));
#9023=DIRECTION('center_axis',(0.,0.,1.));
#9024=DIRECTION('ref_axis',(1.,0.,0.));
#9025=DIRECTION('',(0.,0.,1.));
#9026=DIRECTION('center_axis',(0.,0.,-1.));
#9027=DIRECTION('ref_axis',(1.,0.,0.));
#9028=DIRECTION('',(0.,0.,1.));
#9029=DIRECTION('center_axis',(0.,0.,1.));
#9030=DIRECTION('ref_axis',(1.,0.,0.));
#9031=DIRECTION('center_axis',(0.,0.,1.));
#9032=DIRECTION('ref_axis',(1.,0.,0.));
#9033=DIRECTION('',(0.,0.,1.));
#9034=DIRECTION('center_axis',(0.,0.,1.));
#9035=DIRECTION('ref_axis',(1.,0.,0.));
#9036=DIRECTION('',(0.,0.,1.));
#9037=DIRECTION('center_axis',(0.,0.,-1.));
#9038=DIRECTION('ref_axis',(1.,0.,0.));
#9039=DIRECTION('center_axis',(0.,0.,1.));
#9040=DIRECTION('ref_axis',(1.,0.,0.));
#9041=DIRECTION('center_axis',(0.,0.,1.));
#9042=DIRECTION('ref_axis',(1.,0.,0.));
#9043=DIRECTION('center_axis',(0.,0.,1.));
#9044=DIRECTION('ref_axis',(1.,0.,0.));
#9045=DIRECTION('',(0.,1.,0.));
#9046=DIRECTION('',(-1.,0.,0.));
#9047=DIRECTION('',(0.,-1.,0.));
#9048=DIRECTION('center_axis',(0.,0.,1.));
#9049=DIRECTION('ref_axis',(1.,0.,0.));
#9050=DIRECTION('',(0.,1.,0.));
#9051=DIRECTION('',(0.,-1.,0.));
#9052=DIRECTION('center_axis',(0.,0.,1.));
#9053=DIRECTION('ref_axis',(1.,0.,0.));
#9054=DIRECTION('',(0.,-1.,0.));
#9055=DIRECTION('',(1.,0.,0.));
#9056=DIRECTION('',(0.,1.,0.));
#9057=DIRECTION('center_axis',(0.,0.,1.));
#9058=DIRECTION('ref_axis',(1.,0.,0.));
#9059=DIRECTION('center_axis',(0.,0.,1.));
#9060=DIRECTION('ref_axis',(1.,0.,0.));
#9061=DIRECTION('',(0.,0.,1.));
#9062=DIRECTION('center_axis',(0.,0.,1.));
#9063=DIRECTION('ref_axis',(1.,0.,0.));
#9064=DIRECTION('center_axis',(0.,0.,1.));
#9065=DIRECTION('ref_axis',(1.,0.,0.));
#9066=DIRECTION('',(0.,0.,1.));
#9067=DIRECTION('center_axis',(0.,1.,0.));
#9068=DIRECTION('ref_axis',(-1.,0.,0.));
#9069=DIRECTION('',(-1.,0.,0.));
#9070=DIRECTION('',(0.,0.,1.));
#9071=DIRECTION('',(0.,0.,1.));
#9072=DIRECTION('center_axis',(1.,0.,0.));
#9073=DIRECTION('ref_axis',(0.,1.,0.));
#9074=DIRECTION('',(0.,1.,0.));
#9075=DIRECTION('',(0.,0.,1.));
#9076=DIRECTION('center_axis',(0.,-1.,0.));
#9077=DIRECTION('ref_axis',(1.,0.,0.));
#9078=DIRECTION('',(1.,0.,0.));
#9079=DIRECTION('',(0.,0.,1.));
#9080=DIRECTION('center_axis',(-1.,0.,0.));
#9081=DIRECTION('ref_axis',(0.,-1.,0.));
#9082=DIRECTION('',(0.,-1.,0.));
#9083=DIRECTION('center_axis',(0.,0.,1.));
#9084=DIRECTION('ref_axis',(1.,0.,0.));
#9085=DIRECTION('axis',(0.,0.,1.));
#9086=DIRECTION('refdir',(1.,0.,0.));
#9087=DIRECTION('center_axis',(0.,1.,0.));
#9088=DIRECTION('ref_axis',(-1.,0.,0.));
#9089=DIRECTION('',(-1.,0.,0.));
#9090=DIRECTION('',(0.,0.,1.));
#9091=DIRECTION('',(-1.,0.,0.));
#9092=DIRECTION('',(0.,0.,1.));
#9093=DIRECTION('center_axis',(1.,0.,0.));
#9094=DIRECTION('ref_axis',(0.,1.,0.));
#9095=DIRECTION('',(0.,1.,0.));
#9096=DIRECTION('',(0.,1.,0.));
#9097=DIRECTION('',(0.,0.,1.));
#9098=DIRECTION('center_axis',(0.,-1.,0.));
#9099=DIRECTION('ref_axis',(1.,0.,0.));
#9100=DIRECTION('',(1.,0.,0.));
#9101=DIRECTION('',(1.,0.,0.));
#9102=DIRECTION('',(0.,0.,1.));
#9103=DIRECTION('center_axis',(-1.,0.,0.));
#9104=DIRECTION('ref_axis',(0.,-1.,0.));
#9105=DIRECTION('',(0.,-1.,0.));
#9106=DIRECTION('',(0.,-1.,0.));
#9107=DIRECTION('center_axis',(0.,0.,1.));
#9108=DIRECTION('ref_axis',(1.,0.,0.));
#9109=DIRECTION('center_axis',(0.,0.,1.));
#9110=DIRECTION('ref_axis',(1.,0.,0.));
#9111=DIRECTION('axis',(0.,0.,1.));
#9112=DIRECTION('refdir',(1.,0.,0.));
#9113=DIRECTION('center_axis',(0.,0.,-1.));
#9114=DIRECTION('ref_axis',(0.,1.,0.));
#9115=DIRECTION('',(0.,1.,0.));
#9116=DIRECTION('',(1.,0.,0.));
#9117=DIRECTION('',(0.,-1.,0.));
#9118=DIRECTION('',(1.,0.,0.));
#9119=DIRECTION('center_axis',(0.,1.,-8.88178419700125E-16));
#9120=DIRECTION('ref_axis',(0.,8.88178419700125E-16,1.));
#9121=DIRECTION('',(0.,8.88178419700125E-16,1.));
#9122=DIRECTION('',(1.,0.,0.));
#9123=DIRECTION('',(0.,-8.88178419700125E-16,-1.));
#9124=DIRECTION('center_axis',(0.,-7.40148683083439E-16,-1.));
#9125=DIRECTION('ref_axis',(0.,1.,-7.40148683083439E-16));
#9126=DIRECTION('',(0.,1.,-7.40148683083439E-16));
#9127=DIRECTION('',(1.,0.,0.));
#9128=DIRECTION('',(0.,-1.,7.40148683083439E-16));
#9129=DIRECTION('center_axis',(0.,-0.707106781186547,-0.707106781186548));
#9130=DIRECTION('ref_axis',(0.,0.707106781186548,-0.707106781186547));
#9131=DIRECTION('',(0.,0.707106781186548,-0.707106781186547));
#9132=DIRECTION('',(1.,0.,0.));
#9133=DIRECTION('',(0.,-0.707106781186548,0.707106781186547));
#9134=DIRECTION('center_axis',(0.,-1.,2.77555756156289E-16));
#9135=DIRECTION('ref_axis',(0.,-2.77555756156289E-16,-1.));
#9136=DIRECTION('',(0.,-2.77555756156289E-16,-1.));
#9137=DIRECTION('',(1.,0.,0.));
#9138=DIRECTION('',(0.,2.77555756156289E-16,1.));
#9139=DIRECTION('center_axis',(0.,-0.707106781186547,0.707106781186548));
#9140=DIRECTION('ref_axis',(0.,-0.707106781186548,-0.707106781186547));
#9141=DIRECTION('',(0.,-0.707106781186548,-0.707106781186547));
#9142=DIRECTION('',(1.,0.,0.));
#9143=DIRECTION('',(0.,0.707106781186548,0.707106781186547));
#9144=DIRECTION('center_axis',(0.,7.40148683083438E-16,1.));
#9145=DIRECTION('ref_axis',(0.,-1.,7.40148683083438E-16));
#9146=DIRECTION('',(0.,-1.,7.40148683083438E-16));
#9147=DIRECTION('',(1.,0.,0.));
#9148=DIRECTION('',(0.,1.,-7.40148683083438E-16));
#9149=DIRECTION('center_axis',(0.,1.,-4.44089209850063E-16));
#9150=DIRECTION('ref_axis',(0.,4.44089209850063E-16,1.));
#9151=DIRECTION('',(0.,4.44089209850063E-16,1.));
#9152=DIRECTION('',(1.,0.,0.));
#9153=DIRECTION('',(0.,-4.44089209850063E-16,-1.));
#9154=DIRECTION('center_axis',(0.,2.41352831440251E-16,1.));
#9155=DIRECTION('ref_axis',(0.,-1.,2.41352831440251E-16));
#9156=DIRECTION('',(0.,-1.,2.41352831440251E-16));
#9157=DIRECTION('',(-1.,0.,0.));
#9158=DIRECTION('',(0.,1.,-2.41352831440251E-16));
#9159=DIRECTION('center_axis',(0.,-1.,2.41352831440251E-16));
#9160=DIRECTION('ref_axis',(0.,-2.41352831440251E-16,-1.));
#9161=DIRECTION('',(0.,-2.41352831440251E-16,-1.));
#9162=DIRECTION('',(1.,0.,0.));
#9163=DIRECTION('',(0.,2.41352831440251E-16,1.));
#9164=DIRECTION('',(1.,0.,0.));
#9165=DIRECTION('center_axis',(0.,0.,-1.));
#9166=DIRECTION('ref_axis',(0.,1.,0.));
#9167=DIRECTION('',(0.,1.,0.));
#9168=DIRECTION('',(1.,0.,0.));
#9169=DIRECTION('',(0.,-1.,0.));
#9170=DIRECTION('center_axis',(0.,-1.,0.));
#9171=DIRECTION('ref_axis',(0.,0.,-1.));
#9172=DIRECTION('',(0.,0.,-1.));
#9173=DIRECTION('',(1.,0.,0.));
#9174=DIRECTION('',(0.,0.,1.));
#9175=DIRECTION('center_axis',(0.,-0.707106781186547,0.707106781186548));
#9176=DIRECTION('ref_axis',(0.,-0.707106781186548,-0.707106781186547));
#9177=DIRECTION('',(0.,-0.707106781186548,-0.707106781186547));
#9178=DIRECTION('',(1.,0.,0.));
#9179=DIRECTION('',(0.,0.707106781186548,0.707106781186547));
#9180=DIRECTION('center_axis',(0.,0.,1.));
#9181=DIRECTION('ref_axis',(0.,-1.,0.));
#9182=DIRECTION('',(0.,-1.,0.));
#9183=DIRECTION('',(1.,0.,0.));
#9184=DIRECTION('',(0.,1.,0.));
#9185=DIRECTION('center_axis',(0.,0.707106781186548,0.707106781186547));
#9186=DIRECTION('ref_axis',(0.,-0.707106781186547,0.707106781186548));
#9187=DIRECTION('',(0.,-0.707106781186547,0.707106781186548));
#9188=DIRECTION('',(1.,0.,0.));
#9189=DIRECTION('',(0.,0.707106781186547,-0.707106781186548));
#9190=DIRECTION('center_axis',(0.,1.,0.));
#9191=DIRECTION('ref_axis',(0.,0.,1.));
#9192=DIRECTION('',(0.,0.,1.));
#9193=DIRECTION('',(1.,0.,0.));
#9194=DIRECTION('',(0.,0.,-1.));
#9195=DIRECTION('center_axis',(0.,0.,-1.));
#9196=DIRECTION('ref_axis',(0.,1.,0.));
#9197=DIRECTION('',(0.,1.,0.));
#9198=DIRECTION('',(1.,0.,0.));
#9199=DIRECTION('',(0.,-1.,0.));
#9200=DIRECTION('center_axis',(0.,1.,-2.41352831440251E-16));
#9201=DIRECTION('ref_axis',(0.,2.41352831440251E-16,1.));
#9202=DIRECTION('',(0.,2.41352831440251E-16,1.));
#9203=DIRECTION('',(-1.,0.,0.));
#9204=DIRECTION('',(0.,-2.41352831440251E-16,-1.));
#9205=DIRECTION('center_axis',(0.,0.,1.));
#9206=DIRECTION('ref_axis',(0.,-1.,0.));
#9207=DIRECTION('',(0.,-1.,0.));
#9208=DIRECTION('',(1.,0.,0.));
#9209=DIRECTION('',(0.,1.,0.));
#9210=DIRECTION('',(1.,0.,0.));
#9211=DIRECTION('center_axis',(0.,-1.,0.));
#9212=DIRECTION('ref_axis',(0.,0.,-1.));
#9213=DIRECTION('',(0.,0.,-1.));
#9214=DIRECTION('',(1.,0.,0.));
#9215=DIRECTION('',(0.,0.,1.));
#9216=DIRECTION('center_axis',(0.,0.,1.));
#9217=DIRECTION('ref_axis',(0.,-1.,0.));
#9218=DIRECTION('',(0.,-1.,0.));
#9219=DIRECTION('',(1.,0.,0.));
#9220=DIRECTION('',(0.,1.,0.));
#9221=DIRECTION('center_axis',(0.,0.707106781186548,0.707106781186548));
#9222=DIRECTION('ref_axis',(0.,-0.707106781186548,0.707106781186548));
#9223=DIRECTION('',(0.,-0.707106781186548,0.707106781186548));
#9224=DIRECTION('',(1.,0.,0.));
#9225=DIRECTION('',(0.,0.707106781186548,-0.707106781186548));
#9226=DIRECTION('center_axis',(0.,1.,0.));
#9227=DIRECTION('ref_axis',(0.,0.,1.));
#9228=DIRECTION('',(0.,0.,1.));
#9229=DIRECTION('',(1.,0.,0.));
#9230=DIRECTION('',(0.,0.,-1.));
#9231=DIRECTION('center_axis',(0.,0.707106781186548,-0.707106781186547));
#9232=DIRECTION('ref_axis',(0.,0.707106781186547,0.707106781186548));
#9233=DIRECTION('',(0.,0.707106781186547,0.707106781186548));
#9234=DIRECTION('',(1.,0.,0.));
#9235=DIRECTION('',(0.,-0.707106781186547,-0.707106781186548));
#9236=DIRECTION('center_axis',(0.,-7.40148683083438E-16,-1.));
#9237=DIRECTION('ref_axis',(0.,1.,-7.40148683083438E-16));
#9238=DIRECTION('',(0.,1.,-7.40148683083438E-16));
#9239=DIRECTION('',(1.,0.,0.));
#9240=DIRECTION('',(0.,-1.,7.40148683083438E-16));
#9241=DIRECTION('center_axis',(0.,-1.,0.));
#9242=DIRECTION('ref_axis',(0.,0.,-1.));
#9243=DIRECTION('',(0.,0.,-1.));
#9244=DIRECTION('',(1.,0.,0.));
#9245=DIRECTION('',(0.,0.,1.));
#9246=DIRECTION('center_axis',(0.,0.,-1.));
#9247=DIRECTION('ref_axis',(0.,1.,0.));
#9248=DIRECTION('',(0.,1.,0.));
#9249=DIRECTION('',(-1.,0.,0.));
#9250=DIRECTION('',(0.,-1.,0.));
#9251=DIRECTION('center_axis',(0.,1.,0.));
#9252=DIRECTION('ref_axis',(0.,0.,1.));
#9253=DIRECTION('',(0.,0.,1.));
#9254=DIRECTION('',(1.,0.,0.));
#9255=DIRECTION('',(0.,0.,-1.));
#9256=DIRECTION('',(1.,0.,0.));
#9257=DIRECTION('center_axis',(0.,0.,1.));
#9258=DIRECTION('ref_axis',(0.,-1.,0.));
#9259=DIRECTION('',(0.,-1.,0.));
#9260=DIRECTION('',(1.,0.,0.));
#9261=DIRECTION('',(0.,1.,0.));
#9262=DIRECTION('center_axis',(0.,1.,0.));
#9263=DIRECTION('ref_axis',(0.,0.,1.));
#9264=DIRECTION('',(0.,0.,1.));
#9265=DIRECTION('',(1.,0.,0.));
#9266=DIRECTION('',(0.,0.,-1.));
#9267=DIRECTION('center_axis',(0.,0.707106781186547,-0.707106781186548));
#9268=DIRECTION('ref_axis',(0.,0.707106781186548,0.707106781186547));
#9269=DIRECTION('',(0.,0.707106781186548,0.707106781186547));
#9270=DIRECTION('',(1.,0.,0.));
#9271=DIRECTION('',(0.,-0.707106781186548,-0.707106781186547));
#9272=DIRECTION('center_axis',(0.,0.,-1.));
#9273=DIRECTION('ref_axis',(0.,1.,0.));
#9274=DIRECTION('',(0.,1.,0.));
#9275=DIRECTION('',(1.,0.,0.));
#9276=DIRECTION('',(0.,-1.,0.));
#9277=DIRECTION('center_axis',(0.,-0.707106781186547,-0.707106781186548));
#9278=DIRECTION('ref_axis',(0.,0.707106781186548,-0.707106781186547));
#9279=DIRECTION('',(0.,0.707106781186548,-0.707106781186547));
#9280=DIRECTION('',(1.,0.,0.));
#9281=DIRECTION('',(0.,-0.707106781186548,0.707106781186547));
#9282=DIRECTION('center_axis',(0.,-1.,0.));
#9283=DIRECTION('ref_axis',(0.,0.,-1.));
#9284=DIRECTION('',(0.,0.,-1.));
#9285=DIRECTION('',(1.,0.,0.));
#9286=DIRECTION('',(0.,0.,1.));
#9287=DIRECTION('center_axis',(0.,0.,1.));
#9288=DIRECTION('ref_axis',(0.,-1.,0.));
#9289=DIRECTION('',(0.,-1.,0.));
#9290=DIRECTION('',(1.,0.,0.));
#9291=DIRECTION('',(0.,1.,0.));
#9292=DIRECTION('center_axis',(0.,-1.,0.));
#9293=DIRECTION('ref_axis',(0.,0.,-1.));
#9294=DIRECTION('',(0.,0.,-1.));
#9295=DIRECTION('',(-1.,0.,0.));
#9296=DIRECTION('',(0.,0.,1.));
#9297=DIRECTION('center_axis',(1.,0.,0.));
#9298=DIRECTION('ref_axis',(0.,0.,-1.));
#9299=DIRECTION('center_axis',(1.,0.,0.));
#9300=DIRECTION('ref_axis',(0.,0.,-1.));
#9301=DIRECTION('',(1.,0.,0.));
#9302=DIRECTION('center_axis',(-1.,0.,0.));
#9303=DIRECTION('ref_axis',(0.,0.,-1.));
#9304=DIRECTION('center_axis',(0.,1.,0.));
#9305=DIRECTION('ref_axis',(0.,0.,1.));
#9306=DIRECTION('',(0.,0.,1.));
#9307=DIRECTION('',(1.,0.,0.));
#9308=DIRECTION('',(0.,0.,1.));
#9309=DIRECTION('center_axis',(0.,1.,0.));
#9310=DIRECTION('ref_axis',(0.,0.,1.));
#9311=DIRECTION('',(0.,0.,1.));
#9312=DIRECTION('',(1.,0.,0.));
#9313=DIRECTION('',(0.,0.,1.));
#9314=DIRECTION('center_axis',(0.,0.,-1.));
#9315=DIRECTION('ref_axis',(0.,1.,0.));
#9316=DIRECTION('',(0.,1.,0.));
#9317=DIRECTION('',(0.,1.,0.));
#9318=DIRECTION('center_axis',(0.,0.,-1.));
#9319=DIRECTION('ref_axis',(0.,1.,0.));
#9320=DIRECTION('',(0.,1.,0.));
#9321=DIRECTION('',(1.,0.,0.));
#9322=DIRECTION('',(0.,1.,0.));
#9323=DIRECTION('center_axis',(0.,-1.,0.));
#9324=DIRECTION('ref_axis',(0.,0.,-1.));
#9325=DIRECTION('',(0.,0.,-1.));
#9326=DIRECTION('',(0.,0.,-1.));
#9327=DIRECTION('center_axis',(0.,-1.,0.));
#9328=DIRECTION('ref_axis',(0.,0.,-1.));
#9329=DIRECTION('',(0.,0.,-1.));
#9330=DIRECTION('',(1.,0.,0.));
#9331=DIRECTION('',(0.,0.,-1.));
#9332=DIRECTION('center_axis',(0.,0.,1.));
#9333=DIRECTION('ref_axis',(0.,-1.,0.));
#9334=DIRECTION('',(0.,-1.,0.));
#9335=DIRECTION('',(0.,-1.,0.));
#9336=DIRECTION('center_axis',(0.,0.,1.));
#9337=DIRECTION('ref_axis',(0.,-1.,0.));
#9338=DIRECTION('',(0.,-1.,0.));
#9339=DIRECTION('',(0.,-1.,0.));
#9340=DIRECTION('center_axis',(1.,0.,0.));
#9341=DIRECTION('ref_axis',(0.,0.,-1.));
#9342=DIRECTION('center_axis',(1.,0.,0.));
#9343=DIRECTION('ref_axis',(0.,0.,-1.));
#9344=DIRECTION('axis',(0.,0.,1.));
#9345=DIRECTION('refdir',(1.,0.,0.));
#9346=DIRECTION('center_axis',(0.,0.,1.));
#9347=DIRECTION('ref_axis',(1.,0.,0.));
#9348=DIRECTION('center_axis',(0.,0.,1.));
#9349=DIRECTION('ref_axis',(1.,0.,0.));
#9350=DIRECTION('',(0.,0.,1.));
#9351=DIRECTION('center_axis',(0.,0.,-1.));
#9352=DIRECTION('ref_axis',(1.,0.,0.));
#9353=DIRECTION('center_axis',(0.,0.,1.));
#9354=DIRECTION('ref_axis',(1.,0.,0.));
#9355=DIRECTION('center_axis',(0.,0.,1.));
#9356=DIRECTION('ref_axis',(1.,0.,0.));
#9357=DIRECTION('center_axis',(0.,0.,1.));
#9358=DIRECTION('ref_axis',(1.,0.,0.));
#9359=DIRECTION('center_axis',(0.,0.,1.));
#9360=DIRECTION('ref_axis',(1.,0.,0.));
#9361=DIRECTION('',(0.,0.,1.));
#9362=DIRECTION('center_axis',(0.,0.,-1.));
#9363=DIRECTION('ref_axis',(1.,0.,0.));
#9364=DIRECTION('center_axis',(0.,0.,1.));
#9365=DIRECTION('ref_axis',(1.,0.,0.));
#9366=DIRECTION('center_axis',(0.,0.,1.));
#9367=DIRECTION('ref_axis',(1.,0.,0.));
#9368=DIRECTION('center_axis',(0.,0.,1.));
#9369=DIRECTION('ref_axis',(1.,0.,0.));
#9370=DIRECTION('center_axis',(0.,0.,1.));
#9371=DIRECTION('ref_axis',(1.,0.,0.));
#9372=DIRECTION('',(0.,0.,1.));
#9373=DIRECTION('center_axis',(0.,0.,-1.));
#9374=DIRECTION('ref_axis',(1.,0.,0.));
#9375=DIRECTION('center_axis',(0.,0.,1.));
#9376=DIRECTION('ref_axis',(1.,0.,0.));
#9377=DIRECTION('center_axis',(0.,0.,1.));
#9378=DIRECTION('ref_axis',(1.,0.,0.));
#9379=DIRECTION('center_axis',(0.,0.,1.));
#9380=DIRECTION('ref_axis',(1.,0.,0.));
#9381=DIRECTION('center_axis',(0.,0.,1.));
#9382=DIRECTION('ref_axis',(1.,0.,0.));
#9383=DIRECTION('',(0.,0.,1.));
#9384=DIRECTION('center_axis',(0.,0.,-1.));
#9385=DIRECTION('ref_axis',(1.,0.,0.));
#9386=DIRECTION('center_axis',(0.,0.,1.));
#9387=DIRECTION('ref_axis',(1.,0.,0.));
#9388=DIRECTION('center_axis',(0.,0.,1.));
#9389=DIRECTION('ref_axis',(1.,0.,0.));
#9390=DIRECTION('center_axis',(0.,0.,1.));
#9391=DIRECTION('ref_axis',(1.,0.,0.));
#9392=DIRECTION('center_axis',(0.,0.,1.));
#9393=DIRECTION('ref_axis',(1.,0.,0.));
#9394=DIRECTION('',(0.,0.,1.));
#9395=DIRECTION('center_axis',(0.,0.,1.));
#9396=DIRECTION('ref_axis',(1.,0.,0.));
#9397=DIRECTION('center_axis',(0.,0.,1.));
#9398=DIRECTION('ref_axis',(1.,0.,0.));
#9399=DIRECTION('',(0.,0.,1.));
#9400=DIRECTION('center_axis',(0.,0.,1.));
#9401=DIRECTION('ref_axis',(1.,0.,0.));
#9402=DIRECTION('center_axis',(0.,0.,1.));
#9403=DIRECTION('ref_axis',(1.,0.,0.));
#9404=DIRECTION('',(0.,0.,1.));
#9405=DIRECTION('center_axis',(0.,0.,1.));
#9406=DIRECTION('ref_axis',(1.,0.,0.));
#9407=DIRECTION('center_axis',(0.,0.,1.));
#9408=DIRECTION('ref_axis',(1.,0.,0.));
#9409=DIRECTION('',(0.,0.,1.));
#9410=DIRECTION('center_axis',(0.,-0.56333682464151,0.826227342807548));
#9411=DIRECTION('ref_axis',(0.,-0.826227342807548,-0.56333682464151));
#9412=DIRECTION('',(0.,-0.826227342807548,-0.56333682464151));
#9413=DIRECTION('',(1.,0.,0.));
#9414=DIRECTION('',(0.,-0.826227342807548,-0.56333682464151));
#9415=DIRECTION('',(1.,0.,0.));
#9416=DIRECTION('center_axis',(0.,-1.,0.));
#9417=DIRECTION('ref_axis',(0.,0.,-1.));
#9418=DIRECTION('',(0.,0.,-1.));
#9419=DIRECTION('',(0.,0.,-1.));
#9420=DIRECTION('',(1.,0.,0.));
#9421=DIRECTION('center_axis',(0.,-0.56333682464151,-0.826227342807548));
#9422=DIRECTION('ref_axis',(0.,0.826227342807548,-0.56333682464151));
#9423=DIRECTION('',(0.,0.826227342807548,-0.56333682464151));
#9424=DIRECTION('',(0.,0.826227342807548,-0.56333682464151));
#9425=DIRECTION('',(1.,0.,0.));
#9426=DIRECTION('center_axis',(0.,-1.,0.));
#9427=DIRECTION('ref_axis',(0.,0.,-1.));
#9428=DIRECTION('',(0.,0.,-1.));
#9429=DIRECTION('',(0.,0.,-1.));
#9430=DIRECTION('',(1.,0.,0.));
#9431=DIRECTION('center_axis',(0.,0.,1.));
#9432=DIRECTION('ref_axis',(0.,-1.,0.));
#9433=DIRECTION('',(0.,-1.,0.));
#9434=DIRECTION('',(0.,-1.,0.));
#9435=DIRECTION('',(1.,0.,0.));
#9436=DIRECTION('center_axis',(0.,1.,0.));
#9437=DIRECTION('ref_axis',(0.,0.,1.));
#9438=DIRECTION('',(0.,0.,1.));
#9439=DIRECTION('',(0.,0.,1.));
#9440=DIRECTION('',(1.,0.,0.));
#9441=DIRECTION('center_axis',(0.,0.56333682464151,-0.826227342807548));
#9442=DIRECTION('ref_axis',(0.,0.826227342807548,0.56333682464151));
#9443=DIRECTION('',(0.,0.826227342807548,0.56333682464151));
#9444=DIRECTION('',(0.,0.826227342807548,0.56333682464151));
#9445=DIRECTION('',(1.,0.,0.));
#9446=DIRECTION('center_axis',(0.,1.,0.));
#9447=DIRECTION('ref_axis',(0.,0.,1.));
#9448=DIRECTION('',(0.,0.,1.));
#9449=DIRECTION('',(0.,0.,1.));
#9450=DIRECTION('',(1.,0.,0.));
#9451=DIRECTION('center_axis',(0.,0.56333682464151,0.826227342807548));
#9452=DIRECTION('ref_axis',(0.,-0.826227342807548,0.56333682464151));
#9453=DIRECTION('',(0.,-0.826227342807548,0.56333682464151));
#9454=DIRECTION('',(0.,-0.826227342807548,0.56333682464151));
#9455=DIRECTION('',(1.,0.,0.));
#9456=DIRECTION('center_axis',(0.,1.,0.));
#9457=DIRECTION('ref_axis',(0.,0.,1.));
#9458=DIRECTION('',(0.,0.,1.));
#9459=DIRECTION('',(0.,0.,1.));
#9460=DIRECTION('',(1.,0.,0.));
#9461=DIRECTION('center_axis',(0.,0.,-1.));
#9462=DIRECTION('ref_axis',(0.,1.,0.));
#9463=DIRECTION('',(0.,1.,0.));
#9464=DIRECTION('',(0.,1.,0.));
#9465=DIRECTION('',(1.,0.,0.));
#9466=DIRECTION('center_axis',(0.,-1.,0.));
#9467=DIRECTION('ref_axis',(0.,0.,-1.));
#9468=DIRECTION('',(0.,0.,-1.));
#9469=DIRECTION('',(0.,0.,-1.));
#9470=DIRECTION('center_axis',(1.,0.,0.));
#9471=DIRECTION('ref_axis',(0.,0.,-1.));
#9472=DIRECTION('center_axis',(1.,0.,0.));
#9473=DIRECTION('ref_axis',(0.,0.,-1.));
#9474=DIRECTION('axis',(0.,0.,1.));
#9475=DIRECTION('refdir',(1.,0.,0.));
#9476=DIRECTION('center_axis',(0.,1.,0.));
#9477=DIRECTION('ref_axis',(0.,0.,1.));
#9478=DIRECTION('center_axis',(0.,-1.,0.));
#9479=DIRECTION('ref_axis',(1.,0.,0.));
#9480=DIRECTION('center_axis',(0.,-1.,0.));
#9481=DIRECTION('ref_axis',(1.,0.,0.));
#9482=DIRECTION('center_axis',(0.,-1.,0.));
#9483=DIRECTION('ref_axis',(1.,0.,0.));
#9484=DIRECTION('',(0.707106781186547,0.707106781186548,8.65956056235493E-17));
#9485=DIRECTION('center_axis',(0.,-1.,0.));
#9486=DIRECTION('ref_axis',(1.,0.,0.));
#9487=DIRECTION('center_axis',(0.,-1.,0.));
#9488=DIRECTION('ref_axis',(1.,0.,0.));
#9489=DIRECTION('',(0.,1.,0.));
#9490=DIRECTION('center_axis',(0.,1.,0.));
#9491=DIRECTION('ref_axis',(1.,0.,0.));
#9492=DIRECTION('center_axis',(0.,-1.,0.));
#9493=DIRECTION('ref_axis',(1.,0.,0.));
#9494=DIRECTION('',(-0.707106781186547,0.707106781186548,-8.65956056235493E-17));
#9495=DIRECTION('center_axis',(0.,-1.,0.));
#9496=DIRECTION('ref_axis',(0.,0.,-1.));
#9497=DIRECTION('center_axis',(0.,-1.,0.));
#9498=DIRECTION('ref_axis',(1.,0.,0.));
#9499=DIRECTION('center_axis',(0.,1.,0.));
#9500=DIRECTION('ref_axis',(1.,0.,0.));
#9501=DIRECTION('center_axis',(0.,1.,0.));
#9502=DIRECTION('ref_axis',(1.,0.,0.));
#9503=DIRECTION('',(-0.447213595499958,0.894427190999916,-5.47678698264203E-17));
#9504=DIRECTION('center_axis',(0.,-1.,0.));
#9505=DIRECTION('ref_axis',(1.,0.,0.));
#9506=DIRECTION('center_axis',(0.,1.,0.));
#9507=DIRECTION('ref_axis',(1.,0.,0.));
#9508=DIRECTION('',(0.,1.,0.));
#9509=DIRECTION('center_axis',(0.,1.,0.));
#9510=DIRECTION('ref_axis',(1.,0.,0.));
#9511=DIRECTION('center_axis',(0.,-1.,0.));
#9512=DIRECTION('ref_axis',(1.,0.,0.));
#9513=DIRECTION('',(-0.707106781186547,0.707106781186548,-8.65956056235493E-17));
#9514=DIRECTION('center_axis',(0.,-1.,0.));
#9515=DIRECTION('ref_axis',(0.,0.,-1.));
#9516=DIRECTION('center_axis',(0.866025403784439,0.,-0.5));
#9517=DIRECTION('ref_axis',(0.5,0.,0.866025403784439));
#9518=DIRECTION('',(-0.5,0.,-0.866025403784439));
#9519=DIRECTION('',(0.,-1.,0.));
#9520=DIRECTION('',(0.5,0.,0.866025403784439));
#9521=DIRECTION('',(0.,-1.,0.));
#9522=DIRECTION('center_axis',(1.60246890531964E-16,0.,-1.));
#9523=DIRECTION('ref_axis',(1.,0.,1.60246890531964E-16));
#9524=DIRECTION('',(-1.,0.,-1.60246890531964E-16));
#9525=DIRECTION('',(0.,-1.,0.));
#9526=DIRECTION('',(1.,0.,1.60246890531964E-16));
#9527=DIRECTION('center_axis',(-0.866025403784439,0.,-0.5));
#9528=DIRECTION('ref_axis',(0.5,0.,-0.866025403784439));
#9529=DIRECTION('',(-0.5,0.,0.866025403784439));
#9530=DIRECTION('',(0.,-1.,0.));
#9531=DIRECTION('',(0.5,0.,-0.866025403784439));
#9532=DIRECTION('center_axis',(-0.866025403784439,0.,0.5));
#9533=DIRECTION('ref_axis',(-0.5,0.,-0.866025403784439));
#9534=DIRECTION('',(0.5,0.,0.866025403784439));
#9535=DIRECTION('',(0.,-1.,0.));
#9536=DIRECTION('',(-0.5,0.,-0.866025403784439));
#9537=DIRECTION('center_axis',(-1.60246890531964E-16,0.,1.));
#9538=DIRECTION('ref_axis',(-1.,0.,-1.60246890531964E-16));
#9539=DIRECTION('',(1.,0.,1.60246890531964E-16));
#9540=DIRECTION('',(0.,-1.,0.));
#9541=DIRECTION('',(-1.,0.,-1.60246890531964E-16));
#9542=DIRECTION('center_axis',(0.866025403784439,0.,0.5));
#9543=DIRECTION('ref_axis',(-0.5,0.,0.866025403784439));
#9544=DIRECTION('',(0.5,0.,-0.866025403784439));
#9545=DIRECTION('',(-0.5,0.,0.866025403784439));
#9546=DIRECTION('center_axis',(0.,1.,0.));
#9547=DIRECTION('ref_axis',(1.,0.,0.));
#9548=DIRECTION('center_axis',(0.,-1.,0.));
#9549=DIRECTION('ref_axis',(0.,0.,-1.));
#9550=DIRECTION('axis',(0.,0.,1.));
#9551=DIRECTION('refdir',(1.,0.,0.));
#9552=DIRECTION('center_axis',(0.,0.,1.));
#9553=DIRECTION('ref_axis',(1.,0.,0.));
#9554=DIRECTION('',(1.,0.,0.));
#9555=DIRECTION('',(0.,-1.,0.));
#9556=DIRECTION('',(-1.,0.,0.));
#9557=DIRECTION('',(0.,1.,0.));
#9558=DIRECTION('center_axis',(0.,1.,0.));
#9559=DIRECTION('ref_axis',(-1.,0.,0.));
#9560=DIRECTION('',(0.,0.,1.));
#9561=DIRECTION('',(-1.,0.,0.));
#9562=DIRECTION('',(0.,0.,1.));
#9563=DIRECTION('center_axis',(0.,0.,1.));
#9564=DIRECTION('ref_axis',(1.,0.,0.));
#9565=DIRECTION('',(0.,-1.,0.));
#9566=DIRECTION('',(1.,0.,0.));
#9567=DIRECTION('',(0.,1.,0.));
#9568=DIRECTION('center_axis',(0.,0.,-1.));
#9569=DIRECTION('ref_axis',(1.,0.,0.));
#9570=DIRECTION('center_axis',(-1.,0.,0.));
#9571=DIRECTION('ref_axis',(0.,-1.,0.));
#9572=DIRECTION('',(0.,0.,1.));
#9573=DIRECTION('',(0.,0.707106781186548,0.707106781186548));
#9574=DIRECTION('',(0.,-1.,0.));
#9575=DIRECTION('',(0.,0.707106781186548,-0.707106781186548));
#9576=DIRECTION('',(0.,0.,1.));
#9577=DIRECTION('',(0.,-1.,0.));
#9578=DIRECTION('',(0.,0.,1.));
#9579=DIRECTION('center_axis',(0.,-1.,0.));
#9580=DIRECTION('ref_axis',(1.,0.,0.));
#9581=DIRECTION('',(1.,0.,0.));
#9582=DIRECTION('',(0.,0.,1.));
#9583=DIRECTION('center_axis',(0.,0.,1.));
#9584=DIRECTION('ref_axis',(1.,0.,0.));
#9585=DIRECTION('',(-1.,0.,0.));
#9586=DIRECTION('',(0.,1.,0.));
#9587=DIRECTION('center_axis',(1.,0.,0.));
#9588=DIRECTION('ref_axis',(0.,1.,0.));
#9589=DIRECTION('',(0.,0.,1.));
#9590=DIRECTION('',(0.,-0.707106781186548,0.707106781186548));
#9591=DIRECTION('',(0.,1.,0.));
#9592=DIRECTION('',(0.,-0.707106781186548,-0.707106781186548));
#9593=DIRECTION('',(0.,0.,1.));
#9594=DIRECTION('center_axis',(0.,-1.,0.));
#9595=DIRECTION('ref_axis',(1.,0.,0.));
#9596=DIRECTION('',(-1.,0.,0.));
#9597=DIRECTION('center_axis',(0.,-0.707106781186548,-0.707106781186548));
#9598=DIRECTION('ref_axis',(-1.,0.,0.));
#9599=DIRECTION('',(1.,0.,0.));
#9600=DIRECTION('center_axis',(0.,0.707106781186548,0.707106781186548));
#9601=DIRECTION('ref_axis',(0.,0.707106781186547,-0.707106781186547));
#9602=DIRECTION('',(1.,0.,0.));
#9603=DIRECTION('center_axis',(0.,0.,1.));
#9604=DIRECTION('ref_axis',(1.,0.,0.));
#9605=DIRECTION('center_axis',(0.,0.,-1.));
#9606=DIRECTION('ref_axis',(1.,0.,0.));
#9607=DIRECTION('',(0.,0.,1.));
#9608=DIRECTION('center_axis',(0.,0.,-1.));
#9609=DIRECTION('ref_axis',(1.,0.,0.));
#9610=DIRECTION('center_axis',(0.,-0.707106781186548,0.707106781186548));
#9611=DIRECTION('ref_axis',(0.,0.707106781186547,0.707106781186547));
#9612=DIRECTION('center_axis',(0.,0.,-1.));
#9613=DIRECTION('ref_axis',(1.,0.,0.));
#9614=DIRECTION('center_axis',(0.,0.,1.));
#9615=DIRECTION('ref_axis',(1.,0.,0.));
#9616=DIRECTION('',(-1.,0.,0.));
#9617=DIRECTION('center_axis',(0.,0.,1.));
#9618=DIRECTION('ref_axis',(1.,0.,0.));
#9619=DIRECTION('',(-1.,0.,0.));
#9620=DIRECTION('center_axis',(0.,0.707106781186548,-0.707106781186548));
#9621=DIRECTION('ref_axis',(-1.,0.,0.));
#9622=DIRECTION('',(1.,0.,0.));
#9623=DIRECTION('center_axis',(0.,1.,0.));
#9624=DIRECTION('ref_axis',(-1.,0.,0.));
#9625=DIRECTION('axis',(0.,0.,1.));
#9626=DIRECTION('refdir',(1.,0.,0.));
#9627=DIRECTION('center_axis',(0.866025403784439,0.,-0.5));
#9628=DIRECTION('ref_axis',(0.5,0.,0.866025403784439));
#9629=DIRECTION('',(-0.5,0.,-0.866025403784439));
#9630=DIRECTION('',(0.,-1.,0.));
#9631=DIRECTION('',(0.5,0.,0.866025403784439));
#9632=DIRECTION('',(0.,-1.,0.));
#9633=DIRECTION('center_axis',(1.20185167898973E-16,0.,-1.));
#9634=DIRECTION('ref_axis',(1.,0.,1.20185167898973E-16));
#9635=DIRECTION('',(-1.,0.,-1.20185167898973E-16));
#9636=DIRECTION('',(0.,-1.,0.));
#9637=DIRECTION('',(1.,0.,1.20185167898973E-16));
#9638=DIRECTION('center_axis',(-0.866025403784439,0.,-0.5));
#9639=DIRECTION('ref_axis',(0.5,0.,-0.866025403784439));
#9640=DIRECTION('',(-0.5,0.,0.866025403784439));
#9641=DIRECTION('',(0.,-1.,0.));
#9642=DIRECTION('',(0.5,0.,-0.866025403784439));
#9643=DIRECTION('center_axis',(-0.866025403784439,0.,0.5));
#9644=DIRECTION('ref_axis',(-0.5,0.,-0.866025403784439));
#9645=DIRECTION('',(0.5,0.,0.866025403784439));
#9646=DIRECTION('',(0.,-1.,0.));
#9647=DIRECTION('',(-0.5,0.,-0.866025403784439));
#9648=DIRECTION('center_axis',(-2.40370335797945E-16,0.,1.));
#9649=DIRECTION('ref_axis',(-1.,0.,-2.40370335797945E-16));
#9650=DIRECTION('',(1.,0.,2.40370335797945E-16));
#9651=DIRECTION('',(0.,-1.,0.));
#9652=DIRECTION('',(-1.,0.,-2.40370335797945E-16));
#9653=DIRECTION('center_axis',(0.866025403784439,0.,0.5));
#9654=DIRECTION('ref_axis',(-0.5,0.,0.866025403784439));
#9655=DIRECTION('',(0.5,0.,-0.866025403784439));
#9656=DIRECTION('',(-0.5,0.,0.866025403784439));
#9657=DIRECTION('center_axis',(0.,1.,0.));
#9658=DIRECTION('ref_axis',(1.,0.,0.));
#9659=DIRECTION('center_axis',(0.,-1.,0.));
#9660=DIRECTION('ref_axis',(0.,0.,-1.));
#9661=DIRECTION('center_axis',(0.,1.,0.));
#9662=DIRECTION('ref_axis',(1.,0.,0.));
#9663=DIRECTION('center_axis',(0.,1.,0.));
#9664=DIRECTION('ref_axis',(1.,0.,0.));
#9665=DIRECTION('center_axis',(0.,1.,0.));
#9666=DIRECTION('ref_axis',(0.,0.,1.));
#9667=DIRECTION('center_axis',(0.,-1.,0.));
#9668=DIRECTION('ref_axis',(1.,0.,0.));
#9669=DIRECTION('center_axis',(0.,-1.,0.));
#9670=DIRECTION('ref_axis',(1.,0.,0.));
#9671=DIRECTION('center_axis',(0.,-1.,0.));
#9672=DIRECTION('ref_axis',(1.,0.,0.));
#9673=DIRECTION('',(0.707106781186548,0.707106781186547,8.65956056235493E-17));
#9674=DIRECTION('center_axis',(0.,-1.,0.));
#9675=DIRECTION('ref_axis',(1.,0.,0.));
#9676=DIRECTION('center_axis',(0.,-1.,0.));
#9677=DIRECTION('ref_axis',(1.,0.,0.));
#9678=DIRECTION('',(0.,1.,0.));
#9679=DIRECTION('center_axis',(0.,1.,0.));
#9680=DIRECTION('ref_axis',(1.,0.,0.));
#9681=DIRECTION('center_axis',(0.,-1.,0.));
#9682=DIRECTION('ref_axis',(1.,0.,0.));
#9683=DIRECTION('',(-0.707106781186547,0.707106781186548,-8.65956056235493E-17));
#9684=DIRECTION('center_axis',(0.,-1.,0.));
#9685=DIRECTION('ref_axis',(0.,0.,-1.));
#9686=DIRECTION('center_axis',(0.,-1.,0.));
#9687=DIRECTION('ref_axis',(1.,0.,0.));
#9688=DIRECTION('center_axis',(0.,1.,0.));
#9689=DIRECTION('ref_axis',(1.,0.,0.));
#9690=DIRECTION('center_axis',(0.,1.,0.));
#9691=DIRECTION('ref_axis',(1.,0.,0.));
#9692=DIRECTION('',(-0.447213595499958,0.894427190999916,-5.47678698264203E-17));
#9693=DIRECTION('center_axis',(0.,-1.,0.));
#9694=DIRECTION('ref_axis',(1.,0.,0.));
#9695=DIRECTION('',(0.,1.,0.));
#9696=DIRECTION('axis',(0.,0.,1.));
#9697=DIRECTION('refdir',(1.,0.,0.));
#9698=DIRECTION('axis',(0.,0.,1.));
#9699=DIRECTION('refdir',(1.,0.,0.));
#9700=DIRECTION('center_axis',(0.,0.,1.));
#9701=DIRECTION('ref_axis',(1.,0.,0.));
#9702=DIRECTION('center_axis',(0.,0.,1.));
#9703=DIRECTION('ref_axis',(1.,0.,0.));
#9704=DIRECTION('',(0.,0.,1.));
#9705=DIRECTION('center_axis',(0.,0.,-1.));
#9706=DIRECTION('ref_axis',(1.,0.,0.));
#9707=DIRECTION('center_axis',(0.,0.,1.));
#9708=DIRECTION('ref_axis',(1.,0.,0.));
#9709=DIRECTION('center_axis',(0.,0.,1.));
#9710=DIRECTION('ref_axis',(1.,0.,0.));
#9711=DIRECTION('',(0.,0.,1.));
#9712=DIRECTION('center_axis',(0.,0.,-1.));
#9713=DIRECTION('ref_axis',(1.,0.,0.));
#9714=DIRECTION('center_axis',(0.,0.,1.));
#9715=DIRECTION('ref_axis',(1.,0.,0.));
#9716=DIRECTION('center_axis',(0.,0.,1.));
#9717=DIRECTION('ref_axis',(1.,0.,0.));
#9718=DIRECTION('',(0.,0.,1.));
#9719=DIRECTION('center_axis',(0.,0.,-1.));
#9720=DIRECTION('ref_axis',(1.,0.,0.));
#9721=DIRECTION('center_axis',(0.,0.,1.));
#9722=DIRECTION('ref_axis',(1.,0.,0.));
#9723=DIRECTION('center_axis',(0.,0.,1.));
#9724=DIRECTION('ref_axis',(1.,0.,0.));
#9725=DIRECTION('',(0.,0.,1.));
#9726=DIRECTION('center_axis',(0.,0.,-1.));
#9727=DIRECTION('ref_axis',(1.,0.,0.));
#9728=DIRECTION('center_axis',(0.,0.,1.));
#9729=DIRECTION('ref_axis',(1.,0.,0.));
#9730=DIRECTION('center_axis',(0.,0.,1.));
#9731=DIRECTION('ref_axis',(1.,0.,0.));
#9732=DIRECTION('',(0.,0.,1.));
#9733=DIRECTION('center_axis',(0.,0.,-1.));
#9734=DIRECTION('ref_axis',(1.,0.,0.));
#9735=DIRECTION('center_axis',(0.,0.,1.));
#9736=DIRECTION('ref_axis',(1.,0.,0.));
#9737=DIRECTION('center_axis',(0.,0.,1.));
#9738=DIRECTION('ref_axis',(1.,0.,0.));
#9739=DIRECTION('',(0.,0.,1.));
#9740=DIRECTION('center_axis',(0.,0.,-1.));
#9741=DIRECTION('ref_axis',(1.,0.,0.));
#9742=DIRECTION('center_axis',(0.,0.,1.));
#9743=DIRECTION('ref_axis',(1.,0.,0.));
#9744=DIRECTION('center_axis',(0.,0.,1.));
#9745=DIRECTION('ref_axis',(1.,0.,0.));
#9746=DIRECTION('',(0.,0.,1.));
#9747=DIRECTION('center_axis',(0.,0.,-1.));
#9748=DIRECTION('ref_axis',(1.,0.,0.));
#9749=DIRECTION('center_axis',(0.,0.,1.));
#9750=DIRECTION('ref_axis',(1.,0.,0.));
#9751=DIRECTION('center_axis',(0.,0.,1.));
#9752=DIRECTION('ref_axis',(1.,0.,0.));
#9753=DIRECTION('',(0.,0.,1.));
#9754=DIRECTION('center_axis',(0.,0.,-1.));
#9755=DIRECTION('ref_axis',(1.,0.,0.));
#9756=DIRECTION('center_axis',(0.,0.,1.));
#9757=DIRECTION('ref_axis',(1.,0.,0.));
#9758=DIRECTION('center_axis',(0.,0.,1.));
#9759=DIRECTION('ref_axis',(1.,0.,0.));
#9760=DIRECTION('',(0.,0.,1.));
#9761=DIRECTION('center_axis',(0.,0.,-1.));
#9762=DIRECTION('ref_axis',(1.,0.,0.));
#9763=DIRECTION('center_axis',(0.,0.,1.));
#9764=DIRECTION('ref_axis',(1.,0.,0.));
#9765=DIRECTION('center_axis',(0.,0.,1.));
#9766=DIRECTION('ref_axis',(1.,0.,0.));
#9767=DIRECTION('',(0.,0.,1.));
#9768=DIRECTION('center_axis',(0.,0.,-1.));
#9769=DIRECTION('ref_axis',(1.,0.,0.));
#9770=DIRECTION('center_axis',(0.,0.,1.));
#9771=DIRECTION('ref_axis',(1.,0.,0.));
#9772=DIRECTION('center_axis',(0.,0.,1.));
#9773=DIRECTION('ref_axis',(1.,0.,0.));
#9774=DIRECTION('',(0.,0.,1.));
#9775=DIRECTION('center_axis',(0.,0.,-1.));
#9776=DIRECTION('ref_axis',(1.,0.,0.));
#9777=DIRECTION('center_axis',(0.,0.,1.));
#9778=DIRECTION('ref_axis',(1.,0.,0.));
#9779=DIRECTION('center_axis',(0.,0.,1.));
#9780=DIRECTION('ref_axis',(1.,0.,0.));
#9781=DIRECTION('',(0.,0.,1.));
#9782=DIRECTION('center_axis',(0.,0.,-1.));
#9783=DIRECTION('ref_axis',(1.,0.,0.));
#9784=DIRECTION('center_axis',(0.,0.,1.));
#9785=DIRECTION('ref_axis',(1.,0.,0.));
#9786=DIRECTION('center_axis',(0.,0.,1.));
#9787=DIRECTION('ref_axis',(1.,0.,0.));
#9788=DIRECTION('',(0.,0.,1.));
#9789=DIRECTION('center_axis',(0.,0.,-1.));
#9790=DIRECTION('ref_axis',(1.,0.,0.));
#9791=DIRECTION('center_axis',(0.,0.,1.));
#9792=DIRECTION('ref_axis',(1.,0.,0.));
#9793=DIRECTION('center_axis',(0.,0.,1.));
#9794=DIRECTION('ref_axis',(1.,0.,0.));
#9795=DIRECTION('',(0.,0.,1.));
#9796=DIRECTION('center_axis',(0.,0.,-1.));
#9797=DIRECTION('ref_axis',(1.,0.,0.));
#9798=DIRECTION('center_axis',(0.,0.,1.));
#9799=DIRECTION('ref_axis',(1.,0.,0.));
#9800=DIRECTION('center_axis',(0.,0.,1.));
#9801=DIRECTION('ref_axis',(1.,0.,0.));
#9802=DIRECTION('',(0.,0.,1.));
#9803=DIRECTION('center_axis',(0.,0.,-1.));
#9804=DIRECTION('ref_axis',(1.,0.,0.));
#9805=DIRECTION('center_axis',(0.,0.,1.));
#9806=DIRECTION('ref_axis',(1.,0.,0.));
#9807=DIRECTION('center_axis',(0.,0.,1.));
#9808=DIRECTION('ref_axis',(1.,0.,0.));
#9809=DIRECTION('',(0.,0.,1.));
#9810=DIRECTION('center_axis',(0.,0.,-1.));
#9811=DIRECTION('ref_axis',(1.,0.,0.));
#9812=DIRECTION('center_axis',(0.,0.,1.));
#9813=DIRECTION('ref_axis',(1.,0.,0.));
#9814=DIRECTION('center_axis',(0.,0.,1.));
#9815=DIRECTION('ref_axis',(1.,0.,0.));
#9816=DIRECTION('',(0.,0.,1.));
#9817=DIRECTION('center_axis',(0.,0.,-1.));
#9818=DIRECTION('ref_axis',(1.,0.,0.));
#9819=DIRECTION('center_axis',(0.,0.,1.));
#9820=DIRECTION('ref_axis',(1.,0.,0.));
#9821=DIRECTION('center_axis',(0.,0.,1.));
#9822=DIRECTION('ref_axis',(1.,0.,0.));
#9823=DIRECTION('',(0.,0.,1.));
#9824=DIRECTION('center_axis',(0.,0.,-1.));
#9825=DIRECTION('ref_axis',(1.,0.,0.));
#9826=DIRECTION('center_axis',(0.,0.,1.));
#9827=DIRECTION('ref_axis',(1.,0.,0.));
#9828=DIRECTION('center_axis',(0.,0.,1.));
#9829=DIRECTION('ref_axis',(1.,0.,0.));
#9830=DIRECTION('',(0.,0.,1.));
#9831=DIRECTION('center_axis',(0.,0.,-1.));
#9832=DIRECTION('ref_axis',(1.,0.,0.));
#9833=DIRECTION('center_axis',(0.,1.,0.));
#9834=DIRECTION('ref_axis',(-1.,0.,0.));
#9835=DIRECTION('',(-1.,0.,0.));
#9836=DIRECTION('',(0.,0.,1.));
#9837=DIRECTION('',(-1.,0.,0.));
#9838=DIRECTION('',(0.,0.,1.));
#9839=DIRECTION('center_axis',(1.,0.,0.));
#9840=DIRECTION('ref_axis',(0.,1.,0.));
#9841=DIRECTION('',(0.,1.,0.));
#9842=DIRECTION('',(0.,1.,0.));
#9843=DIRECTION('',(0.,0.,1.));
#9844=DIRECTION('center_axis',(0.,-1.,0.));
#9845=DIRECTION('ref_axis',(1.,0.,0.));
#9846=DIRECTION('',(1.,0.,0.));
#9847=DIRECTION('',(1.,0.,0.));
#9848=DIRECTION('',(0.,0.,1.));
#9849=DIRECTION('center_axis',(-1.,0.,0.));
#9850=DIRECTION('ref_axis',(0.,-1.,0.));
#9851=DIRECTION('',(0.,-1.,0.));
#9852=DIRECTION('',(0.,-1.,0.));
#9853=DIRECTION('center_axis',(0.,0.,1.));
#9854=DIRECTION('ref_axis',(1.,0.,0.));
#9855=DIRECTION('center_axis',(0.,0.,1.));
#9856=DIRECTION('ref_axis',(1.,0.,0.));
#9857=DIRECTION('axis',(0.,0.,1.));
#9858=DIRECTION('refdir',(1.,0.,0.));
#9859=DIRECTION('center_axis',(0.,0.,1.));
#9860=DIRECTION('ref_axis',(1.,0.,0.));
#9861=DIRECTION('center_axis',(0.,0.,-1.));
#9862=DIRECTION('ref_axis',(1.,0.,0.));
#9863=DIRECTION('',(0.,0.,-1.));
#9864=DIRECTION('center_axis',(0.,0.,-1.));
#9865=DIRECTION('ref_axis',(1.,0.,0.));
#9866=DIRECTION('center_axis',(0.,0.,1.));
#9867=DIRECTION('ref_axis',(1.,0.,0.));
#9868=DIRECTION('center_axis',(0.,0.,1.));
#9869=DIRECTION('ref_axis',(1.,0.,0.));
#9870=DIRECTION('',(0.,0.,-1.));
#9871=DIRECTION('center_axis',(0.,0.,1.));
#9872=DIRECTION('ref_axis',(1.,0.,0.));
#9873=DIRECTION('center_axis',(0.,0.,1.));
#9874=DIRECTION('ref_axis',(1.,0.,0.));
#9875=DIRECTION('center_axis',(0.,0.,1.));
#9876=DIRECTION('ref_axis',(1.,0.,0.));
#9877=DIRECTION('axis',(0.,0.,1.));
#9878=DIRECTION('refdir',(1.,0.,0.));
#9879=DIRECTION('center_axis',(0.,0.,1.));
#9880=DIRECTION('ref_axis',(1.,0.,0.));
#9881=DIRECTION('center_axis',(0.,0.,1.));
#9882=DIRECTION('ref_axis',(1.,0.,0.));
#9883=DIRECTION('',(0.,0.,1.));
#9884=DIRECTION('center_axis',(0.,0.,-1.));
#9885=DIRECTION('ref_axis',(1.,0.,0.));
#9886=DIRECTION('center_axis',(0.,0.,1.));
#9887=DIRECTION('ref_axis',(1.,0.,0.));
#9888=DIRECTION('center_axis',(0.,0.,1.));
#9889=DIRECTION('ref_axis',(1.,0.,0.));
#9890=DIRECTION('',(0.,0.,1.));
#9891=DIRECTION('center_axis',(0.,0.,-1.));
#9892=DIRECTION('ref_axis',(1.,0.,0.));
#9893=DIRECTION('center_axis',(0.,0.,1.));
#9894=DIRECTION('ref_axis',(0.,-1.,0.));
#9895=DIRECTION('',(0.,-1.,0.));
#9896=DIRECTION('',(1.,0.,0.));
#9897=DIRECTION('',(0.,-1.,0.));
#9898=DIRECTION('',(1.,0.,0.));
#9899=DIRECTION('center_axis',(0.,-1.,0.));
#9900=DIRECTION('ref_axis',(0.,0.,-1.));
#9901=DIRECTION('',(0.,0.,-1.));
#9902=DIRECTION('',(0.,0.,-1.));
#9903=DIRECTION('',(1.,0.,0.));
#9904=DIRECTION('center_axis',(0.,0.,1.));
#9905=DIRECTION('ref_axis',(0.,-1.,0.));
#9906=DIRECTION('',(0.,-1.,0.));
#9907=DIRECTION('',(0.,-1.,0.));
#9908=DIRECTION('',(1.,0.,0.));
#9909=DIRECTION('center_axis',(0.,1.,0.));
#9910=DIRECTION('ref_axis',(0.,0.,1.));
#9911=DIRECTION('',(0.,0.,1.));
#9912=DIRECTION('',(0.,0.,1.));
#9913=DIRECTION('',(1.,0.,0.));
#9914=DIRECTION('center_axis',(0.,0.,-1.));
#9915=DIRECTION('ref_axis',(0.,1.,0.));
#9916=DIRECTION('',(0.,1.,0.));
#9917=DIRECTION('',(0.,1.,0.));
#9918=DIRECTION('',(1.,0.,0.));
#9919=DIRECTION('center_axis',(0.,-1.,0.));
#9920=DIRECTION('ref_axis',(0.,0.,-1.));
#9921=DIRECTION('',(0.,0.,-1.));
#9922=DIRECTION('',(0.,0.,-1.));
#9923=DIRECTION('center_axis',(1.,0.,0.));
#9924=DIRECTION('ref_axis',(0.,0.,-1.));
#9925=DIRECTION('center_axis',(1.,0.,0.));
#9926=DIRECTION('ref_axis',(0.,0.,-1.));
#9927=DIRECTION('axis',(0.,0.,1.));
#9928=DIRECTION('refdir',(1.,0.,0.));
#9929=DIRECTION('axis',(0.,0.,1.));
#9930=DIRECTION('refdir',(1.,0.,0.));
#9931=DIRECTION('center_axis',(0.,0.,1.));
#9932=DIRECTION('ref_axis',(1.,0.,0.));
#9933=DIRECTION('',(-1.,0.,0.));
#9934=DIRECTION('center_axis',(0.,0.,1.));
#9935=DIRECTION('ref_axis',(1.,0.,0.));
#9936=DIRECTION('center_axis',(0.,0.,1.));
#9937=DIRECTION('ref_axis',(1.,0.,0.));
#9938=DIRECTION('',(0.,0.,-1.));
#9939=DIRECTION('center_axis',(0.,0.,1.));
#9940=DIRECTION('ref_axis',(1.,0.,0.));
#9941=DIRECTION('',(0.,0.,1.));
#9942=DIRECTION('center_axis',(0.,0.,-1.));
#9943=DIRECTION('ref_axis',(1.,0.,0.));
#9944=DIRECTION('center_axis',(0.,0.,1.));
#9945=DIRECTION('ref_axis',(1.,0.,0.));
#9946=DIRECTION('',(0.,0.,1.));
#9947=DIRECTION('center_axis',(0.,0.,1.));
#9948=DIRECTION('ref_axis',(1.,0.,0.));
#9949=DIRECTION('',(1.,0.,0.));
#9950=DIRECTION('center_axis',(0.,0.,1.));
#9951=DIRECTION('ref_axis',(1.,0.,0.));
#9952=DIRECTION('center_axis',(0.,0.,1.));
#9953=DIRECTION('ref_axis',(1.,0.,0.));
#9954=DIRECTION('',(0.,0.,-1.));
#9955=DIRECTION('center_axis',(0.,0.,1.));
#9956=DIRECTION('ref_axis',(1.,0.,0.));
#9957=DIRECTION('',(0.,0.,1.));
#9958=DIRECTION('center_axis',(0.,0.,-1.));
#9959=DIRECTION('ref_axis',(1.,0.,0.));
#9960=DIRECTION('center_axis',(0.,0.,1.));
#9961=DIRECTION('ref_axis',(1.,0.,0.));
#9962=DIRECTION('',(0.,0.,1.));
#9963=DIRECTION('center_axis',(0.,0.,1.));
#9964=DIRECTION('ref_axis',(1.,0.,0.));
#9965=DIRECTION('',(-1.,0.,0.));
#9966=DIRECTION('center_axis',(0.,0.,1.));
#9967=DIRECTION('ref_axis',(1.,0.,0.));
#9968=DIRECTION('center_axis',(0.,0.,1.));
#9969=DIRECTION('ref_axis',(1.,0.,0.));
#9970=DIRECTION('',(0.,0.,-1.));
#9971=DIRECTION('center_axis',(0.,0.,1.));
#9972=DIRECTION('ref_axis',(1.,0.,0.));
#9973=DIRECTION('',(0.,0.,1.));
#9974=DIRECTION('center_axis',(0.,0.,-1.));
#9975=DIRECTION('ref_axis',(1.,0.,0.));
#9976=DIRECTION('center_axis',(0.,0.,1.));
#9977=DIRECTION('ref_axis',(1.,0.,0.));
#9978=DIRECTION('',(0.,0.,1.));
#9979=DIRECTION('center_axis',(0.,0.,1.));
#9980=DIRECTION('ref_axis',(1.,0.,0.));
#9981=DIRECTION('',(1.,0.,0.));
#9982=DIRECTION('center_axis',(0.,0.,1.));
#9983=DIRECTION('ref_axis',(1.,0.,0.));
#9984=DIRECTION('center_axis',(0.,0.,1.));
#9985=DIRECTION('ref_axis',(1.,0.,0.));
#9986=DIRECTION('',(0.,0.,-1.));
#9987=DIRECTION('center_axis',(0.,0.,1.));
#9988=DIRECTION('ref_axis',(1.,0.,0.));
#9989=DIRECTION('',(0.,0.,1.));
#9990=DIRECTION('center_axis',(0.,0.,-1.));
#9991=DIRECTION('ref_axis',(1.,0.,0.));
#9992=DIRECTION('center_axis',(0.,0.,1.));
#9993=DIRECTION('ref_axis',(1.,0.,0.));
#9994=DIRECTION('',(0.,0.,1.));
#9995=DIRECTION('center_axis',(0.,-1.,0.));
#9996=DIRECTION('ref_axis',(0.,0.,-1.));
#9997=DIRECTION('',(-1.,0.,0.));
#9998=DIRECTION('',(-1.,0.,0.));
#9999=DIRECTION('',(0.,0.,1.));
#10000=DIRECTION('',(1.,0.,0.));
#10001=DIRECTION('',(0.,0.,-1.));
#10002=DIRECTION('',(-1.,0.,0.));
#10003=DIRECTION('center_axis',(0.,1.,0.));
#10004=DIRECTION('ref_axis',(0.,0.,1.));
#10005=DIRECTION('',(1.,0.,0.));
#10006=DIRECTION('',(1.,0.,0.));
#10007=DIRECTION('',(0.,0.,1.));
#10008=DIRECTION('',(1.,0.,0.));
#10009=DIRECTION('',(0.,0.,-1.));
#10010=DIRECTION('',(1.,0.,0.));
#10011=DIRECTION('center_axis',(-1.,0.,0.));
#10012=DIRECTION('ref_axis',(0.,0.,1.));
#10013=DIRECTION('',(0.,-1.,0.));
#10014=DIRECTION('',(0.,0.,1.));
#10015=DIRECTION('',(0.,1.,0.));
#10016=DIRECTION('',(0.,0.,-1.));
#10017=DIRECTION('',(0.,-1.,0.));
#10018=DIRECTION('',(0.,-1.,0.));
#10019=DIRECTION('',(0.,0.,1.));
#10020=DIRECTION('',(0.,-1.,0.));
#10021=DIRECTION('',(0.,0.,-1.));
#10022=DIRECTION('',(0.,-1.,0.));
#10023=DIRECTION('center_axis',(0.,0.,-1.));
#10024=DIRECTION('ref_axis',(0.,1.,0.));
#10025=DIRECTION('',(0.,1.,0.));
#10026=DIRECTION('',(1.,0.,0.));
#10027=DIRECTION('center_axis',(0.,-1.,0.));
#10028=DIRECTION('ref_axis',(0.,0.,-1.));
#10029=DIRECTION('',(0.,0.,-1.));
#10030=DIRECTION('',(1.,0.,0.));
#10031=DIRECTION('center_axis',(0.,0.,1.));
#10032=DIRECTION('ref_axis',(0.,-1.,0.));
#10033=DIRECTION('',(0.,-1.,0.));
#10034=DIRECTION('',(1.,0.,0.));
#10035=DIRECTION('center_axis',(0.,1.,0.));
#10036=DIRECTION('ref_axis',(0.,0.,1.));
#10037=DIRECTION('',(0.,0.,1.));
#10038=DIRECTION('',(1.,0.,0.));
#10039=DIRECTION('center_axis',(0.,0.,-1.));
#10040=DIRECTION('ref_axis',(0.,1.,0.));
#10041=DIRECTION('',(0.,1.,0.));
#10042=DIRECTION('center_axis',(0.,0.,-1.));
#10043=DIRECTION('ref_axis',(0.,1.,0.));
#10044=DIRECTION('',(0.,1.,0.));
#10045=DIRECTION('',(1.,0.,0.));
#10046=DIRECTION('center_axis',(0.,-1.,0.));
#10047=DIRECTION('ref_axis',(0.,0.,-1.));
#10048=DIRECTION('',(0.,0.,-1.));
#10049=DIRECTION('',(1.,0.,0.));
#10050=DIRECTION('center_axis',(0.,0.,-1.));
#10051=DIRECTION('ref_axis',(0.,1.,0.));
#10052=DIRECTION('',(0.,1.,0.));
#10053=DIRECTION('',(1.,0.,0.));
#10054=DIRECTION('center_axis',(0.,1.,0.));
#10055=DIRECTION('ref_axis',(0.,0.,1.));
#10056=DIRECTION('',(0.,0.,1.));
#10057=DIRECTION('',(1.,0.,0.));
#10058=DIRECTION('center_axis',(0.,0.,-1.));
#10059=DIRECTION('ref_axis',(0.,1.,0.));
#10060=DIRECTION('',(0.,1.,0.));
#10061=DIRECTION('center_axis',(1.,0.,0.));
#10062=DIRECTION('ref_axis',(0.,0.,-1.));
#10063=DIRECTION('axis',(0.,0.,1.));
#10064=DIRECTION('refdir',(1.,0.,0.));
#10065=DIRECTION('center_axis',(0.,0.,1.));
#10066=DIRECTION('ref_axis',(0.,-1.,0.));
#10067=DIRECTION('',(0.,-1.,0.));
#10068=DIRECTION('',(1.,0.,0.));
#10069=DIRECTION('',(0.,-1.,0.));
#10070=DIRECTION('',(1.,0.,0.));
#10071=DIRECTION('center_axis',(0.,1.,0.));
#10072=DIRECTION('ref_axis',(0.,0.,1.));
#10073=DIRECTION('',(0.,0.,1.));
#10074=DIRECTION('',(0.,0.,1.));
#10075=DIRECTION('',(1.,0.,0.));
#10076=DIRECTION('center_axis',(0.,0.,-1.));
#10077=DIRECTION('ref_axis',(0.,1.,0.));
#10078=DIRECTION('',(0.,1.,0.));
#10079=DIRECTION('',(0.,1.,0.));
#10080=DIRECTION('',(1.,0.,0.));
#10081=DIRECTION('center_axis',(0.,-1.,0.));
#10082=DIRECTION('ref_axis',(0.,0.,-1.));
#10083=DIRECTION('',(0.,0.,-1.));
#10084=DIRECTION('',(0.,0.,-1.));
#10085=DIRECTION('',(1.,0.,0.));
#10086=DIRECTION('center_axis',(0.,0.,-1.));
#10087=DIRECTION('ref_axis',(0.,1.,0.));
#10088=DIRECTION('',(0.,1.,0.));
#10089=DIRECTION('',(0.,1.,0.));
#10090=DIRECTION('',(1.,0.,0.));
#10091=DIRECTION('center_axis',(0.,1.,0.));
#10092=DIRECTION('ref_axis',(0.,0.,1.));
#10093=DIRECTION('',(0.,0.,1.));
#10094=DIRECTION('',(0.,0.,1.));
#10095=DIRECTION('',(1.,0.,0.));
#10096=DIRECTION('center_axis',(0.,0.,-1.));
#10097=DIRECTION('ref_axis',(0.,1.,0.));
#10098=DIRECTION('',(0.,1.,0.));
#10099=DIRECTION('',(0.,1.,0.));
#10100=DIRECTION('',(1.,0.,0.));
#10101=DIRECTION('center_axis',(0.,-1.,0.));
#10102=DIRECTION('ref_axis',(0.,0.,-1.));
#10103=DIRECTION('',(0.,0.,-1.));
#10104=DIRECTION('',(0.,0.,-1.));
#10105=DIRECTION('center_axis',(1.,0.,0.));
#10106=DIRECTION('ref_axis',(0.,0.,-1.));
#10107=DIRECTION('center_axis',(1.,0.,0.));
#10108=DIRECTION('ref_axis',(0.,0.,-1.));
#10109=DIRECTION('axis',(0.,0.,1.));
#10110=DIRECTION('refdir',(1.,0.,0.));
#10111=DIRECTION('center_axis',(0.,0.,-1.));
#10112=DIRECTION('ref_axis',(0.,-1.,0.));
#10113=DIRECTION('',(0.,1.,0.));
#10114=DIRECTION('',(-1.,0.,0.));
#10115=DIRECTION('',(0.,-1.,0.));
#10116=DIRECTION('',(-1.,0.,0.));
#10117=DIRECTION('center_axis',(0.,1.,0.));
#10118=DIRECTION('ref_axis',(0.,0.,-1.));
#10119=DIRECTION('',(0.,0.,1.));
#10120=DIRECTION('',(0.,0.,-1.));
#10121=DIRECTION('',(-1.,0.,0.));
#10122=DIRECTION('center_axis',(0.,0.,-1.));
#10123=DIRECTION('ref_axis',(0.,-1.,0.));
#10124=DIRECTION('',(0.,1.,0.));
#10125=DIRECTION('',(0.,-1.,0.));
#10126=DIRECTION('',(-1.,0.,0.));
#10127=DIRECTION('center_axis',(0.,-1.,0.));
#10128=DIRECTION('ref_axis',(0.,0.,1.));
#10129=DIRECTION('',(0.,0.,-1.));
#10130=DIRECTION('',(0.,0.,1.));
#10131=DIRECTION('',(-1.,0.,0.));
#10132=DIRECTION('center_axis',(0.,0.,-1.));
#10133=DIRECTION('ref_axis',(0.,-1.,0.));
#10134=DIRECTION('',(0.,1.,0.));
#10135=DIRECTION('',(0.,-1.,0.));
#10136=DIRECTION('',(-1.,0.,0.));
#10137=DIRECTION('center_axis',(0.,1.,0.));
#10138=DIRECTION('ref_axis',(0.,0.,-1.));
#10139=DIRECTION('',(0.,0.,1.));
#10140=DIRECTION('',(0.,0.,-1.));
#10141=DIRECTION('',(-1.,0.,0.));
#10142=DIRECTION('center_axis',(0.,0.,1.));
#10143=DIRECTION('ref_axis',(0.,1.,0.));
#10144=DIRECTION('',(0.,-1.,0.));
#10145=DIRECTION('',(0.,1.,0.));
#10146=DIRECTION('',(-1.,0.,0.));
#10147=DIRECTION('center_axis',(0.,-1.,0.));
#10148=DIRECTION('ref_axis',(0.,0.,1.));
#10149=DIRECTION('',(0.,0.,-1.));
#10150=DIRECTION('',(0.,0.,1.));
#10151=DIRECTION('center_axis',(1.,0.,0.));
#10152=DIRECTION('ref_axis',(0.,0.,-1.));
#10153=DIRECTION('center_axis',(-1.,0.,0.));
#10154=DIRECTION('ref_axis',(0.,0.,1.));
#10155=DIRECTION('',(0.,0.,1.));
#10156=DIRECTION('',(1.,0.,0.));
#10157=DIRECTION('',(0.,0.,1.));
#10158=DIRECTION('',(1.,0.,0.));
#10159=DIRECTION('',(0.,0.,1.));
#10160=DIRECTION('',(1.,0.,0.));
#10161=DIRECTION('axis',(0.,0.,1.));
#10162=DIRECTION('refdir',(1.,0.,0.));
#10163=DIRECTION('center_axis',(0.,1.,0.));
#10164=DIRECTION('ref_axis',(1.,0.,0.));
#10165=DIRECTION('center_axis',(0.,1.,0.));
#10166=DIRECTION('ref_axis',(1.,0.,0.));
#10167=DIRECTION('',(0.707106781186548,-0.707106781186547,-8.65956056235494E-17));
#10168=DIRECTION('center_axis',(0.,-1.,0.));
#10169=DIRECTION('ref_axis',(1.,0.,0.));
#10170=DIRECTION('center_axis',(0.,1.,0.));
#10171=DIRECTION('ref_axis',(1.,0.,0.));
#10172=DIRECTION('',(0.,-1.,0.));
#10173=DIRECTION('center_axis',(0.,-1.,0.));
#10174=DIRECTION('ref_axis',(1.,0.,0.));
#10175=DIRECTION('center_axis',(0.,1.,0.));
#10176=DIRECTION('ref_axis',(1.,0.,0.));
#10177=DIRECTION('center_axis',(0.,1.,0.));
#10178=DIRECTION('ref_axis',(1.,0.,0.));
#10179=DIRECTION('center_axis',(0.,1.,0.));
#10180=DIRECTION('ref_axis',(1.,0.,0.));
#10181=DIRECTION('',(0.,-1.,0.));
#10182=DIRECTION('center_axis',(0.,1.,0.));
#10183=DIRECTION('ref_axis',(1.,0.,0.));
#10184=DIRECTION('center_axis',(0.,1.,0.));
#10185=DIRECTION('ref_axis',(1.,0.,0.));
#10186=DIRECTION('',(0.,0.,1.));
#10187=DIRECTION('',(1.,0.,0.));
#10188=DIRECTION('',(0.,0.,1.));
#10189=DIRECTION('',(1.,0.,0.));
#10190=DIRECTION('',(0.,0.,1.));
#10191=DIRECTION('',(1.,0.,0.));
#10192=DIRECTION('',(0.,0.,1.));
#10193=DIRECTION('',(1.,0.,0.));
#10194=DIRECTION('',(0.,0.,1.));
#10195=DIRECTION('',(1.,0.,0.));
#10196=DIRECTION('',(0.,0.,1.));
#10197=DIRECTION('',(1.,0.,0.));
#10198=DIRECTION('',(0.,0.,1.));
#10199=DIRECTION('',(1.,0.,0.));
#10200=DIRECTION('',(0.,0.,1.));
#10201=DIRECTION('',(1.,0.,0.));
#10202=DIRECTION('',(0.,0.,1.));
#10203=DIRECTION('',(1.,0.,0.));
#10204=DIRECTION('',(0.,0.,1.));
#10205=DIRECTION('',(1.,0.,0.));
#10206=DIRECTION('',(0.,0.,1.));
#10207=DIRECTION('',(1.,0.,0.));
#10208=DIRECTION('',(0.,0.,1.));
#10209=DIRECTION('',(1.,0.,0.));
#10210=DIRECTION('',(0.,0.,1.));
#10211=DIRECTION('',(1.,0.,0.));
#10212=DIRECTION('',(0.,0.,1.));
#10213=DIRECTION('',(1.,0.,0.));
#10214=DIRECTION('',(0.,0.,1.));
#10215=DIRECTION('',(1.,0.,0.));
#10216=DIRECTION('',(0.,0.,1.));
#10217=DIRECTION('',(1.,0.,0.));
#10218=DIRECTION('',(0.,-1.,2.22044604925031E-16));
#10219=DIRECTION('',(1.,0.,0.));
#10220=DIRECTION('',(0.,-1.,2.22044604925031E-16));
#10221=DIRECTION('',(1.,0.,0.));
#10222=DIRECTION('',(0.,0.,1.));
#10223=DIRECTION('',(1.,0.,0.));
#10224=DIRECTION('',(0.,-1.,2.22044604925031E-16));
#10225=DIRECTION('',(1.,0.,0.));
#10226=DIRECTION('',(0.,-1.,2.22044604925031E-16));
#10227=DIRECTION('',(1.,0.,0.));
#10228=DIRECTION('',(0.,0.,1.));
#10229=DIRECTION('',(1.,0.,0.));
#10230=DIRECTION('',(0.,-1.,2.22044604925031E-16));
#10231=DIRECTION('',(1.,0.,0.));
#10232=DIRECTION('',(0.,-1.,2.22044604925031E-16));
#10233=DIRECTION('',(1.,0.,0.));
#10234=DIRECTION('',(0.,-1.,2.22044604925031E-16));
#10235=DIRECTION('',(1.,0.,0.));
#10236=DIRECTION('',(0.,-1.,2.22044604925031E-16));
#10237=DIRECTION('',(1.,0.,0.));
#10238=DIRECTION('',(0.,0.,1.));
#10239=DIRECTION('',(1.,0.,0.));
#10240=DIRECTION('',(0.,0.,1.));
#10241=DIRECTION('',(1.,0.,0.));
#10242=DIRECTION('',(0.,-1.,2.22044604925031E-16));
#10243=DIRECTION('',(1.,0.,0.));
#10244=DIRECTION('',(0.,-1.,2.22044604925031E-16));
#10245=DIRECTION('',(1.,0.,0.));
#10246=DIRECTION('',(0.,0.,1.));
#10247=DIRECTION('',(1.,0.,0.));
#10248=DIRECTION('',(0.,-1.,2.22044604925031E-16));
#10249=DIRECTION('',(1.,0.,0.));
#10250=DIRECTION('',(0.,-1.,2.22044604925031E-16));
#10251=DIRECTION('',(1.,0.,0.));
#10252=DIRECTION('',(0.,0.,1.));
#10253=DIRECTION('',(1.,0.,0.));
#10254=DIRECTION('',(0.,-1.,2.22044604925031E-16));
#10255=DIRECTION('',(1.,0.,0.));
#10256=DIRECTION('',(0.,-1.,2.22044604925031E-16));
#10257=DIRECTION('',(1.,0.,0.));
#10258=DIRECTION('',(0.,-1.,2.22044604925031E-16));
#10259=DIRECTION('',(1.,0.,0.));
#10260=DIRECTION('',(0.,-1.,2.22044604925031E-16));
#10261=DIRECTION('',(1.,0.,0.));
#10262=DIRECTION('',(0.,0.,1.));
#10263=DIRECTION('',(1.,0.,0.));
#10264=DIRECTION('',(0.,-1.,2.22044604925031E-16));
#10265=DIRECTION('',(1.,0.,0.));
#10266=DIRECTION('',(0.,-1.,2.22044604925031E-16));
#10267=DIRECTION('',(1.,0.,0.));
#10268=DIRECTION('',(0.,-1.22464679914735E-16,-1.));
#10269=DIRECTION('',(1.,0.,0.));
#10270=DIRECTION('',(0.,1.,2.22044604925031E-16));
#10271=DIRECTION('',(1.,0.,0.));
#10272=DIRECTION('',(0.,1.,2.22044604925031E-16));
#10273=DIRECTION('',(1.,0.,0.));
#10274=DIRECTION('',(0.,0.,1.));
#10275=DIRECTION('',(1.,0.,0.));
#10276=DIRECTION('',(0.,-1.,2.22044604925031E-16));
#10277=DIRECTION('',(1.,0.,0.));
#10278=DIRECTION('',(0.,-1.,2.22044604925031E-16));
#10279=DIRECTION('',(1.,0.,0.));
#10280=DIRECTION('',(0.,-1.22464679914735E-16,-1.));
#10281=DIRECTION('',(1.,0.,0.));
#10282=DIRECTION('',(0.,1.,2.22044604925031E-16));
#10283=DIRECTION('',(1.,0.,0.));
#10284=DIRECTION('',(0.,1.,2.22044604925031E-16));
#10285=DIRECTION('',(1.,0.,0.));
#10286=DIRECTION('',(0.,0.,1.));
#10287=DIRECTION('',(1.,0.,0.));
#10288=DIRECTION('',(0.,-1.,2.22044604925031E-16));
#10289=DIRECTION('',(1.,0.,0.));
#10290=DIRECTION('',(0.,-1.,2.22044604925031E-16));
#10291=DIRECTION('',(1.,0.,0.));
#10292=DIRECTION('',(0.,-1.22464679914735E-16,-1.));
#10293=DIRECTION('',(1.,0.,0.));
#10294=DIRECTION('',(0.,1.,2.22044604925031E-16));
#10295=DIRECTION('',(1.,0.,0.));
#10296=DIRECTION('',(0.,1.,2.22044604925031E-16));
#10297=DIRECTION('',(1.,0.,0.));
#10298=DIRECTION('',(0.,0.,1.));
#10299=DIRECTION('',(1.,0.,0.));
#10300=DIRECTION('',(0.,-1.,2.22044604925031E-16));
#10301=DIRECTION('',(1.,0.,0.));
#10302=DIRECTION('',(0.,-1.,2.22044604925031E-16));
#10303=DIRECTION('',(1.,0.,0.));
#10304=DIRECTION('',(0.,-1.22464679914735E-16,-1.));
#10305=DIRECTION('',(1.,0.,0.));
#10306=DIRECTION('',(0.,1.,2.22044604925031E-16));
#10307=DIRECTION('',(1.,0.,0.));
#10308=DIRECTION('',(0.,1.,2.22044604925031E-16));
#10309=DIRECTION('',(1.,0.,0.));
#10310=DIRECTION('',(0.,0.,1.));
#10311=DIRECTION('',(1.,0.,0.));
#10312=DIRECTION('',(0.,-1.,2.22044604925031E-16));
#10313=DIRECTION('',(1.,0.,0.));
#10314=DIRECTION('',(0.,0.,1.));
#10315=DIRECTION('',(1.,0.,0.));
#10316=DIRECTION('',(0.,-1.,2.22044604925031E-16));
#10317=DIRECTION('',(1.,0.,0.));
#10318=DIRECTION('',(0.,0.,1.));
#10319=DIRECTION('',(1.,0.,0.));
#10320=DIRECTION('',(0.,-1.,2.22044604925031E-16));
#10321=DIRECTION('',(1.,0.,0.));
#10322=DIRECTION('',(0.,0.,1.));
#10323=DIRECTION('',(1.,0.,0.));
#10324=DIRECTION('',(0.,-1.,2.22044604925031E-16));
#10325=DIRECTION('',(1.,0.,0.));
#10326=DIRECTION('axis',(0.,0.,1.));
#10327=DIRECTION('refdir',(1.,0.,0.));
#10328=DIRECTION('center_axis',(0.,1.,0.));
#10329=DIRECTION('ref_axis',(0.,0.,1.));
#10330=DIRECTION('center_axis',(0.,-1.,0.));
#10331=DIRECTION('ref_axis',(1.,0.,0.));
#10332=DIRECTION('center_axis',(0.,-1.,0.));
#10333=DIRECTION('ref_axis',(1.,0.,0.));
#10334=DIRECTION('center_axis',(0.,-1.,0.));
#10335=DIRECTION('ref_axis',(1.,0.,0.));
#10336=DIRECTION('',(0.707106781186548,0.707106781186547,8.65956056235493E-17));
#10337=DIRECTION('center_axis',(0.,-1.,0.));
#10338=DIRECTION('ref_axis',(1.,0.,0.));
#10339=DIRECTION('center_axis',(0.,-1.,0.));
#10340=DIRECTION('ref_axis',(1.,0.,0.));
#10341=DIRECTION('',(0.,1.,0.));
#10342=DIRECTION('center_axis',(0.,1.,0.));
#10343=DIRECTION('ref_axis',(1.,0.,0.));
#10344=DIRECTION('center_axis',(0.,-1.,0.));
#10345=DIRECTION('ref_axis',(1.,0.,0.));
#10346=DIRECTION('',(-0.707106781186547,0.707106781186548,-8.65956056235493E-17));
#10347=DIRECTION('center_axis',(0.,-1.,0.));
#10348=DIRECTION('ref_axis',(0.,0.,-1.));
#10349=DIRECTION('center_axis',(0.,-1.,0.));
#10350=DIRECTION('ref_axis',(1.,0.,0.));
#10351=DIRECTION('center_axis',(0.,1.,0.));
#10352=DIRECTION('ref_axis',(1.,0.,0.));
#10353=DIRECTION('center_axis',(0.,1.,0.));
#10354=DIRECTION('ref_axis',(1.,0.,0.));
#10355=DIRECTION('',(-0.447213595499958,0.894427190999916,-5.47678698264203E-17));
#10356=DIRECTION('center_axis',(0.,-1.,0.));
#10357=DIRECTION('ref_axis',(1.,0.,0.));
#10358=DIRECTION('center_axis',(0.,1.,0.));
#10359=DIRECTION('ref_axis',(1.,0.,0.));
#10360=DIRECTION('',(0.,1.,0.));
#10361=DIRECTION('center_axis',(0.,1.,0.));
#10362=DIRECTION('ref_axis',(1.,0.,0.));
#10363=DIRECTION('center_axis',(0.,-1.,0.));
#10364=DIRECTION('ref_axis',(1.,0.,0.));
#10365=DIRECTION('',(-0.707106781186547,0.707106781186548,-8.65956056235493E-17));
#10366=DIRECTION('center_axis',(0.,-1.,0.));
#10367=DIRECTION('ref_axis',(0.,0.,-1.));
#10368=DIRECTION('center_axis',(0.866025403784439,0.,-0.5));
#10369=DIRECTION('ref_axis',(0.5,0.,0.866025403784439));
#10370=DIRECTION('',(-0.5,0.,-0.866025403784439));
#10371=DIRECTION('',(0.,-1.,0.));
#10372=DIRECTION('',(0.5,0.,0.866025403784439));
#10373=DIRECTION('',(0.,-1.,0.));
#10374=DIRECTION('center_axis',(1.20185167898973E-16,0.,-1.));
#10375=DIRECTION('ref_axis',(1.,0.,1.20185167898973E-16));
#10376=DIRECTION('',(-1.,0.,-1.20185167898973E-16));
#10377=DIRECTION('',(0.,-1.,0.));
#10378=DIRECTION('',(1.,0.,1.20185167898973E-16));
#10379=DIRECTION('center_axis',(-0.866025403784439,0.,-0.5));
#10380=DIRECTION('ref_axis',(0.5,0.,-0.866025403784439));
#10381=DIRECTION('',(-0.5,0.,0.866025403784439));
#10382=DIRECTION('',(0.,-1.,0.));
#10383=DIRECTION('',(0.5,0.,-0.866025403784439));
#10384=DIRECTION('center_axis',(-0.866025403784439,0.,0.5));
#10385=DIRECTION('ref_axis',(-0.5,0.,-0.866025403784439));
#10386=DIRECTION('',(0.5,0.,0.866025403784439));
#10387=DIRECTION('',(0.,-1.,0.));
#10388=DIRECTION('',(-0.5,0.,-0.866025403784439));
#10389=DIRECTION('center_axis',(-2.40370335797945E-16,0.,1.));
#10390=DIRECTION('ref_axis',(-1.,0.,-2.40370335797945E-16));
#10391=DIRECTION('',(1.,0.,2.40370335797945E-16));
#10392=DIRECTION('',(0.,-1.,0.));
#10393=DIRECTION('',(-1.,0.,-2.40370335797945E-16));
#10394=DIRECTION('center_axis',(0.866025403784439,0.,0.5));
#10395=DIRECTION('ref_axis',(-0.5,0.,0.866025403784439));
#10396=DIRECTION('',(0.5,0.,-0.866025403784439));
#10397=DIRECTION('',(-0.5,0.,0.866025403784439));
#10398=DIRECTION('center_axis',(0.,1.,0.));
#10399=DIRECTION('ref_axis',(1.,0.,0.));
#10400=DIRECTION('center_axis',(0.,-1.,0.));
#10401=DIRECTION('ref_axis',(0.,0.,-1.));
#10402=DIRECTION('axis',(0.,0.,1.));
#10403=DIRECTION('refdir',(1.,0.,0.));
#10404=DIRECTION('center_axis',(0.,1.,0.));
#10405=DIRECTION('ref_axis',(1.,0.,0.));
#10406=DIRECTION('center_axis',(0.,-1.,0.));
#10407=DIRECTION('ref_axis',(1.,0.,0.));
#10408=DIRECTION('',(0.,-1.,0.));
#10409=DIRECTION('center_axis',(0.,-1.,0.));
#10410=DIRECTION('ref_axis',(1.,0.,0.));
#10411=DIRECTION('center_axis',(0.,1.,0.));
#10412=DIRECTION('ref_axis',(1.,0.,0.));
#10413=DIRECTION('center_axis',(0.,1.,0.));
#10414=DIRECTION('ref_axis',(1.,0.,0.));
#10415=DIRECTION('',(0.,-1.,0.));
#10416=DIRECTION('center_axis',(0.,1.,0.));
#10417=DIRECTION('ref_axis',(1.,0.,0.));
#10418=DIRECTION('center_axis',(0.,1.,0.));
#10419=DIRECTION('ref_axis',(1.,0.,0.));
#10420=DIRECTION('center_axis',(0.,1.,0.));
#10421=DIRECTION('ref_axis',(1.,0.,0.));
#10422=DIRECTION('axis',(0.,0.,1.));
#10423=DIRECTION('refdir',(1.,0.,0.));
#10424=DIRECTION('center_axis',(0.,1.,0.));
#10425=DIRECTION('ref_axis',(0.,0.,1.));
#10426=DIRECTION('center_axis',(0.,-1.,0.));
#10427=DIRECTION('ref_axis',(1.,0.,0.));
#10428=DIRECTION('center_axis',(0.,-1.,0.));
#10429=DIRECTION('ref_axis',(1.,0.,0.));
#10430=DIRECTION('center_axis',(0.,-1.,0.));
#10431=DIRECTION('ref_axis',(1.,0.,0.));
#10432=DIRECTION('',(0.707106781186548,0.707106781186547,8.65956056235494E-17));
#10433=DIRECTION('center_axis',(0.,-1.,0.));
#10434=DIRECTION('ref_axis',(1.,0.,0.));
#10435=DIRECTION('center_axis',(0.,-1.,0.));
#10436=DIRECTION('ref_axis',(1.,0.,0.));
#10437=DIRECTION('',(0.,1.,0.));
#10438=DIRECTION('center_axis',(0.,1.,0.));
#10439=DIRECTION('ref_axis',(1.,0.,0.));
#10440=DIRECTION('center_axis',(0.,-1.,0.));
#10441=DIRECTION('ref_axis',(1.,0.,0.));
#10442=DIRECTION('',(-0.707106781186547,0.707106781186548,-8.65956056235493E-17));
#10443=DIRECTION('center_axis',(0.,-1.,0.));
#10444=DIRECTION('ref_axis',(0.,0.,-1.));
#10445=DIRECTION('center_axis',(0.,-1.,0.));
#10446=DIRECTION('ref_axis',(1.,0.,0.));
#10447=DIRECTION('center_axis',(0.,1.,0.));
#10448=DIRECTION('ref_axis',(1.,0.,0.));
#10449=DIRECTION('center_axis',(0.,1.,0.));
#10450=DIRECTION('ref_axis',(1.,0.,0.));
#10451=DIRECTION('',(-0.447213595499958,0.894427190999916,-5.47678698264203E-17));
#10452=DIRECTION('center_axis',(0.,-1.,0.));
#10453=DIRECTION('ref_axis',(1.,0.,0.));
#10454=DIRECTION('center_axis',(0.,1.,0.));
#10455=DIRECTION('ref_axis',(1.,0.,0.));
#10456=DIRECTION('',(0.,1.,0.));
#10457=DIRECTION('center_axis',(0.,1.,0.));
#10458=DIRECTION('ref_axis',(1.,0.,0.));
#10459=DIRECTION('center_axis',(0.,-1.,0.));
#10460=DIRECTION('ref_axis',(1.,0.,0.));
#10461=DIRECTION('',(-0.707106781186547,0.707106781186548,-8.65956056235493E-17));
#10462=DIRECTION('center_axis',(0.,-1.,0.));
#10463=DIRECTION('ref_axis',(0.,0.,-1.));
#10464=DIRECTION('center_axis',(0.866025403784439,0.,-0.5));
#10465=DIRECTION('ref_axis',(0.5,0.,0.866025403784439));
#10466=DIRECTION('',(-0.5,0.,-0.866025403784439));
#10467=DIRECTION('',(0.,-1.,0.));
#10468=DIRECTION('',(0.5,0.,0.866025403784439));
#10469=DIRECTION('',(0.,-1.,0.));
#10470=DIRECTION('center_axis',(1.92296268638356E-16,0.,-1.));
#10471=DIRECTION('ref_axis',(1.,0.,1.92296268638356E-16));
#10472=DIRECTION('',(-1.,0.,-1.92296268638356E-16));
#10473=DIRECTION('',(0.,-1.,0.));
#10474=DIRECTION('',(1.,0.,1.92296268638356E-16));
#10475=DIRECTION('center_axis',(-0.866025403784439,0.,-0.5));
#10476=DIRECTION('ref_axis',(0.5,0.,-0.866025403784439));
#10477=DIRECTION('',(-0.5,0.,0.866025403784438));
#10478=DIRECTION('',(0.,-1.,0.));
#10479=DIRECTION('',(0.5,0.,-0.866025403784438));
#10480=DIRECTION('center_axis',(-0.866025403784439,0.,0.5));
#10481=DIRECTION('ref_axis',(-0.5,0.,-0.866025403784439));
#10482=DIRECTION('',(0.5,0.,0.866025403784439));
#10483=DIRECTION('',(0.,-1.,0.));
#10484=DIRECTION('',(-0.5,0.,-0.866025403784439));
#10485=DIRECTION('center_axis',(-1.92296268638356E-16,0.,1.));
#10486=DIRECTION('ref_axis',(-1.,0.,-1.92296268638356E-16));
#10487=DIRECTION('',(1.,0.,1.92296268638356E-16));
#10488=DIRECTION('',(0.,-1.,0.));
#10489=DIRECTION('',(-1.,0.,-1.92296268638356E-16));
#10490=DIRECTION('center_axis',(0.866025403784439,0.,0.5));
#10491=DIRECTION('ref_axis',(-0.5,0.,0.866025403784439));
#10492=DIRECTION('',(0.5,0.,-0.866025403784439));
#10493=DIRECTION('',(-0.5,0.,0.866025403784439));
#10494=DIRECTION('center_axis',(0.,1.,0.));
#10495=DIRECTION('ref_axis',(1.,0.,0.));
#10496=DIRECTION('center_axis',(0.,-1.,0.));
#10497=DIRECTION('ref_axis',(0.,0.,-1.));
#10498=DIRECTION('axis',(0.,0.,1.));
#10499=DIRECTION('refdir',(1.,0.,0.));
#10500=DIRECTION('center_axis',(0.,1.,0.));
#10501=DIRECTION('ref_axis',(1.,0.,0.));
#10502=DIRECTION('center_axis',(0.,1.,0.));
#10503=DIRECTION('ref_axis',(1.,0.,0.));
#10504=DIRECTION('',(0.707106781186547,-0.707106781186548,-8.65956056235493E-17));
#10505=DIRECTION('center_axis',(0.,-1.,0.));
#10506=DIRECTION('ref_axis',(1.,0.,0.));
#10507=DIRECTION('center_axis',(0.,1.,0.));
#10508=DIRECTION('ref_axis',(1.,0.,0.));
#10509=DIRECTION('',(0.,-1.,0.));
#10510=DIRECTION('center_axis',(0.,-1.,0.));
#10511=DIRECTION('ref_axis',(1.,0.,0.));
#10512=DIRECTION('center_axis',(0.,1.,0.));
#10513=DIRECTION('ref_axis',(1.,0.,0.));
#10514=DIRECTION('center_axis',(0.,1.,0.));
#10515=DIRECTION('ref_axis',(1.,0.,0.));
#10516=DIRECTION('center_axis',(0.,1.,0.));
#10517=DIRECTION('ref_axis',(1.,0.,0.));
#10518=DIRECTION('',(0.,-1.,0.));
#10519=DIRECTION('center_axis',(0.,1.,0.));
#10520=DIRECTION('ref_axis',(1.,0.,0.));
#10521=DIRECTION('center_axis',(0.,1.,0.));
#10522=DIRECTION('ref_axis',(1.,0.,0.));
#10523=DIRECTION('axis',(0.,0.,1.));
#10524=DIRECTION('refdir',(1.,0.,0.));
#10525=DIRECTION('center_axis',(0.866025403784439,0.,-0.5));
#10526=DIRECTION('ref_axis',(0.5,0.,0.866025403784439));
#10527=DIRECTION('',(-0.5,0.,-0.866025403784439));
#10528=DIRECTION('',(0.,-1.,0.));
#10529=DIRECTION('',(0.5,0.,0.866025403784439));
#10530=DIRECTION('',(0.,-1.,0.));
#10531=DIRECTION('center_axis',(1.60246890531964E-16,0.,-1.));
#10532=DIRECTION('ref_axis',(1.,0.,1.60246890531964E-16));
#10533=DIRECTION('',(-1.,0.,-1.60246890531964E-16));
#10534=DIRECTION('',(0.,-1.,0.));
#10535=DIRECTION('',(1.,0.,1.60246890531964E-16));
#10536=DIRECTION('center_axis',(-0.866025403784439,0.,-0.5));
#10537=DIRECTION('ref_axis',(0.5,0.,-0.866025403784439));
#10538=DIRECTION('',(-0.5,0.,0.866025403784439));
#10539=DIRECTION('',(0.,-1.,0.));
#10540=DIRECTION('',(0.5,0.,-0.866025403784439));
#10541=DIRECTION('center_axis',(-0.866025403784439,0.,0.5));
#10542=DIRECTION('ref_axis',(-0.5,0.,-0.866025403784439));
#10543=DIRECTION('',(0.5,0.,0.866025403784439));
#10544=DIRECTION('',(0.,-1.,0.));
#10545=DIRECTION('',(-0.5,0.,-0.866025403784439));
#10546=DIRECTION('center_axis',(-1.60246890531964E-16,0.,1.));
#10547=DIRECTION('ref_axis',(-1.,0.,-1.60246890531964E-16));
#10548=DIRECTION('',(1.,0.,1.60246890531964E-16));
#10549=DIRECTION('',(0.,-1.,0.));
#10550=DIRECTION('',(-1.,0.,-1.60246890531964E-16));
#10551=DIRECTION('center_axis',(0.866025403784439,0.,0.5));
#10552=DIRECTION('ref_axis',(-0.5,0.,0.866025403784439));
#10553=DIRECTION('',(0.5,0.,-0.866025403784439));
#10554=DIRECTION('',(-0.5,0.,0.866025403784439));
#10555=DIRECTION('center_axis',(0.,1.,0.));
#10556=DIRECTION('ref_axis',(1.,0.,0.));
#10557=DIRECTION('center_axis',(0.,-1.,0.));
#10558=DIRECTION('ref_axis',(0.,0.,-1.));
#10559=DIRECTION('center_axis',(0.,1.,0.));
#10560=DIRECTION('ref_axis',(1.,0.,0.));
#10561=DIRECTION('center_axis',(0.,1.,0.));
#10562=DIRECTION('ref_axis',(1.,0.,0.));
#10563=DIRECTION('center_axis',(0.,1.,0.));
#10564=DIRECTION('ref_axis',(0.,0.,1.));
#10565=DIRECTION('center_axis',(0.,-1.,0.));
#10566=DIRECTION('ref_axis',(1.,0.,0.));
#10567=DIRECTION('center_axis',(0.,-1.,0.));
#10568=DIRECTION('ref_axis',(1.,0.,0.));
#10569=DIRECTION('center_axis',(0.,-1.,0.));
#10570=DIRECTION('ref_axis',(1.,0.,0.));
#10571=DIRECTION('',(0.707106781186547,0.707106781186548,8.65956056235493E-17));
#10572=DIRECTION('center_axis',(0.,-1.,0.));
#10573=DIRECTION('ref_axis',(1.,0.,0.));
#10574=DIRECTION('center_axis',(0.,-1.,0.));
#10575=DIRECTION('ref_axis',(1.,0.,0.));
#10576=DIRECTION('',(0.,1.,0.));
#10577=DIRECTION('center_axis',(0.,1.,0.));
#10578=DIRECTION('ref_axis',(1.,0.,0.));
#10579=DIRECTION('center_axis',(0.,-1.,0.));
#10580=DIRECTION('ref_axis',(1.,0.,0.));
#10581=DIRECTION('',(-0.707106781186547,0.707106781186548,-8.65956056235493E-17));
#10582=DIRECTION('center_axis',(0.,-1.,0.));
#10583=DIRECTION('ref_axis',(0.,0.,-1.));
#10584=DIRECTION('center_axis',(0.,-1.,0.));
#10585=DIRECTION('ref_axis',(1.,0.,0.));
#10586=DIRECTION('center_axis',(0.,1.,0.));
#10587=DIRECTION('ref_axis',(1.,0.,0.));
#10588=DIRECTION('center_axis',(0.,1.,0.));
#10589=DIRECTION('ref_axis',(1.,0.,0.));
#10590=DIRECTION('',(-0.447213595499958,0.894427190999916,-5.47678698264203E-17));
#10591=DIRECTION('center_axis',(0.,-1.,0.));
#10592=DIRECTION('ref_axis',(1.,0.,0.));
#10593=DIRECTION('',(0.,1.,0.));
#10594=DIRECTION('',(0.,0.,1.));
#10595=DIRECTION('',(1.,0.,0.));
#10596=DIRECTION('',(0.,0.,1.));
#10597=DIRECTION('',(1.,0.,0.));
#10598=DIRECTION('',(0.,0.,1.));
#10599=DIRECTION('',(1.,0.,0.));
#10600=DIRECTION('',(0.,0.,1.));
#10601=DIRECTION('',(1.,0.,0.));
#10602=DIRECTION('',(0.,0.,1.));
#10603=DIRECTION('',(1.,0.,0.));
#10604=DIRECTION('',(0.,0.,1.));
#10605=DIRECTION('',(1.,0.,0.));
#10606=DIRECTION('',(0.,0.,1.));
#10607=DIRECTION('',(1.,0.,0.));
#10608=DIRECTION('',(0.,-1.,2.22044604925031E-16));
#10609=DIRECTION('',(1.,0.,0.));
#10610=DIRECTION('',(0.,-1.,2.22044604925031E-16));
#10611=DIRECTION('',(1.,0.,0.));
#10612=DIRECTION('',(0.,-1.,2.22044604925031E-16));
#10613=DIRECTION('',(1.,0.,0.));
#10614=DIRECTION('',(0.,-1.,2.22044604925031E-16));
#10615=DIRECTION('',(1.,0.,0.));
#10616=DIRECTION('',(0.,-1.,2.22044604925031E-16));
#10617=DIRECTION('',(1.,0.,0.));
#10618=DIRECTION('',(0.,-1.,2.22044604925031E-16));
#10619=DIRECTION('',(1.,0.,0.));
#10620=DIRECTION('',(0.,-1.,2.22044604925031E-16));
#10621=DIRECTION('',(1.,0.,0.));
#10622=DIRECTION('',(0.,-1.,2.22044604925031E-16));
#10623=DIRECTION('',(1.,0.,0.));
#10624=DIRECTION('',(0.,-1.,2.22044604925031E-16));
#10625=DIRECTION('',(1.,0.,0.));
#10626=DIRECTION('',(0.,-1.,2.22044604925031E-16));
#10627=DIRECTION('',(1.,0.,0.));
#10628=DIRECTION('',(0.,-1.,2.22044604925031E-16));
#10629=DIRECTION('',(1.,0.,0.));
#10630=DIRECTION('',(0.,-1.,2.22044604925031E-16));
#10631=DIRECTION('',(1.,0.,0.));
#10632=DIRECTION('',(0.,-1.,2.22044604925031E-16));
#10633=DIRECTION('',(1.,0.,0.));
#10634=DIRECTION('',(0.,-1.,2.22044604925031E-16));
#10635=DIRECTION('',(1.,0.,0.));
#10636=DIRECTION('',(0.,-1.,2.22044604925031E-16));
#10637=DIRECTION('',(1.,0.,0.));
#10638=DIRECTION('',(0.,-1.,2.22044604925031E-16));
#10639=DIRECTION('',(1.,0.,0.));
#10640=DIRECTION('',(0.,-1.,2.22044604925031E-16));
#10641=DIRECTION('',(1.,0.,0.));
#10642=DIRECTION('',(0.,-1.,2.22044604925031E-16));
#10643=DIRECTION('',(1.,0.,0.));
#10644=DIRECTION('',(0.,-1.,2.22044604925031E-16));
#10645=DIRECTION('',(1.,0.,0.));
#10646=DIRECTION('',(0.,-1.,2.22044604925031E-16));
#10647=DIRECTION('',(1.,0.,0.));
#10648=DIRECTION('',(0.,-1.,2.22044604925031E-16));
#10649=DIRECTION('',(1.,0.,0.));
#10650=DIRECTION('',(0.,-1.,2.22044604925031E-16));
#10651=DIRECTION('',(1.,0.,0.));
#10652=DIRECTION('',(0.,-1.,2.22044604925031E-16));
#10653=DIRECTION('',(1.,0.,0.));
#10654=DIRECTION('',(0.,-1.,2.22044604925031E-16));
#10655=DIRECTION('',(1.,0.,0.));
#10656=DIRECTION('',(0.,-1.,2.22044604925031E-16));
#10657=DIRECTION('',(1.,0.,0.));
#10658=DIRECTION('',(0.,-1.,2.22044604925031E-16));
#10659=DIRECTION('',(1.,0.,0.));
#10660=DIRECTION('',(0.,-1.,2.22044604925031E-16));
#10661=DIRECTION('',(1.,0.,0.));
#10662=DIRECTION('',(0.,-1.,2.22044604925031E-16));
#10663=DIRECTION('',(1.,0.,0.));
#10664=DIRECTION('',(0.,-1.,2.22044604925031E-16));
#10665=DIRECTION('',(1.,0.,0.));
#10666=DIRECTION('',(0.,-1.,2.22044604925031E-16));
#10667=DIRECTION('',(1.,0.,0.));
#10668=DIRECTION('',(0.,-1.,2.22044604925031E-16));
#10669=DIRECTION('',(1.,0.,0.));
#10670=DIRECTION('',(0.,-1.,2.22044604925031E-16));
#10671=DIRECTION('',(1.,0.,0.));
#10672=DIRECTION('',(0.,-1.,2.22044604925031E-16));
#10673=DIRECTION('',(1.,0.,0.));
#10674=DIRECTION('',(0.,-1.,2.22044604925031E-16));
#10675=DIRECTION('',(1.,0.,0.));
#10676=DIRECTION('',(0.,-1.,2.22044604925031E-16));
#10677=DIRECTION('',(1.,0.,0.));
#10678=DIRECTION('',(0.,-1.,2.22044604925031E-16));
#10679=DIRECTION('',(1.,0.,0.));
#10680=DIRECTION('',(0.,-1.,2.22044604925031E-16));
#10681=DIRECTION('',(1.,0.,0.));
#10682=DIRECTION('',(0.,-1.,2.22044604925031E-16));
#10683=DIRECTION('',(1.,0.,0.));
#10684=DIRECTION('',(0.,0.,1.));
#10685=DIRECTION('',(1.,0.,0.));
#10686=DIRECTION('',(0.,0.,1.));
#10687=DIRECTION('',(1.,0.,0.));
#10688=CARTESIAN_POINT('',(0.,0.,0.));
#10689=CARTESIAN_POINT('',(0.,0.,0.));
#10690=CARTESIAN_POINT('',(0.,0.,0.));
#10691=CARTESIAN_POINT('Origin',(23.,-10.,1.9));
#10692=CARTESIAN_POINT('',(22.835,-10.,2.));
#10693=CARTESIAN_POINT('Origin',(23.,-10.,2.));
#10694=CARTESIAN_POINT('',(22.835,-10.,2.8));
#10695=CARTESIAN_POINT('',(22.835,-10.,1.9));
#10696=CARTESIAN_POINT('Origin',(23.,-10.,2.8));
#10697=CARTESIAN_POINT('Origin',(17.,-10.,1.9));
#10698=CARTESIAN_POINT('',(16.835,-10.,2.));
#10699=CARTESIAN_POINT('Origin',(17.,-10.,2.));
#10700=CARTESIAN_POINT('',(16.835,-10.,2.8));
#10701=CARTESIAN_POINT('',(16.835,-10.,1.9));
#10702=CARTESIAN_POINT('Origin',(17.,-10.,2.8));
#10703=CARTESIAN_POINT('Origin',(11.,-10.,1.9));
#10704=CARTESIAN_POINT('',(10.835,-10.,2.));
#10705=CARTESIAN_POINT('Origin',(11.,-10.,2.));
#10706=CARTESIAN_POINT('',(10.835,-10.,2.8));
#10707=CARTESIAN_POINT('',(10.835,-10.,1.9));
#10708=CARTESIAN_POINT('Origin',(11.,-10.,2.8));
#10709=CARTESIAN_POINT('Origin',(29.,-10.,1.9));
#10710=CARTESIAN_POINT('',(28.835,-10.,2.));
#10711=CARTESIAN_POINT('Origin',(29.,-10.,2.));
#10712=CARTESIAN_POINT('',(28.835,-10.,2.8));
#10713=CARTESIAN_POINT('',(28.835,-10.,1.9));
#10714=CARTESIAN_POINT('Origin',(29.,-10.,2.8));
#10715=CARTESIAN_POINT('Origin',(8.5,-10.,1.9));
#10716=CARTESIAN_POINT('',(8.225,-10.,2.));
#10717=CARTESIAN_POINT('Origin',(8.5,-10.,2.));
#10718=CARTESIAN_POINT('',(8.225,-10.,2.8));
#10719=CARTESIAN_POINT('',(8.225,-10.,1.9));
#10720=CARTESIAN_POINT('Origin',(8.5,-10.,2.8));
#10721=CARTESIAN_POINT('Origin',(31.5,-10.,1.9));
#10722=CARTESIAN_POINT('',(31.225,-10.,2.));
#10723=CARTESIAN_POINT('Origin',(31.5,-10.,2.));
#10724=CARTESIAN_POINT('',(31.225,-10.,2.8));
#10725=CARTESIAN_POINT('',(31.225,-10.,1.9));
#10726=CARTESIAN_POINT('Origin',(31.5,-10.,2.8));
#10727=CARTESIAN_POINT('Origin',(32.,-7.5,2.));
#10728=CARTESIAN_POINT('',(32.,-7.5,2.));
#10729=CARTESIAN_POINT('',(8.,-7.5,2.));
#10730=CARTESIAN_POINT('',(32.,-7.5,2.));
#10731=CARTESIAN_POINT('',(8.,-7.5,2.8));
#10732=CARTESIAN_POINT('',(8.,-7.5,2.));
#10733=CARTESIAN_POINT('',(32.,-7.5,2.8));
#10734=CARTESIAN_POINT('',(32.,-7.5,2.8));
#10735=CARTESIAN_POINT('',(32.,-7.5,2.));
#10736=CARTESIAN_POINT('Origin',(32.,-12.5,2.));
#10737=CARTESIAN_POINT('',(32.,-12.5,2.));
#10738=CARTESIAN_POINT('',(32.,-12.5,2.));
#10739=CARTESIAN_POINT('',(32.,-12.5,2.8));
#10740=CARTESIAN_POINT('',(32.,-12.5,2.8));
#10741=CARTESIAN_POINT('',(32.,-12.5,2.));
#10742=CARTESIAN_POINT('Origin',(8.,-12.5,2.));
#10743=CARTESIAN_POINT('',(8.,-12.5,2.));
#10744=CARTESIAN_POINT('',(8.,-12.5,2.));
#10745=CARTESIAN_POINT('',(8.,-12.5,2.8));
#10746=CARTESIAN_POINT('',(8.,-12.5,2.8));
#10747=CARTESIAN_POINT('',(8.,-12.5,2.));
#10748=CARTESIAN_POINT('Origin',(8.,-7.5,2.));
#10749=CARTESIAN_POINT('',(8.,-7.5,2.));
#10750=CARTESIAN_POINT('',(8.,-7.5,2.8));
#10751=CARTESIAN_POINT('Origin',(20.,-10.,2.8));
#10752=CARTESIAN_POINT('Origin',(20.,-10.,2.));
#10753=CARTESIAN_POINT('',(0.,0.,0.));
#10754=CARTESIAN_POINT('Origin',(23.,10.,1.9));
#10755=CARTESIAN_POINT('',(22.835,10.,2.));
#10756=CARTESIAN_POINT('Origin',(23.,10.,2.));
#10757=CARTESIAN_POINT('',(22.835,10.,2.8));
#10758=CARTESIAN_POINT('',(22.835,10.,1.9));
#10759=CARTESIAN_POINT('Origin',(23.,10.,2.8));
#10760=CARTESIAN_POINT('Origin',(17.,10.,1.9));
#10761=CARTESIAN_POINT('',(16.835,10.,2.));
#10762=CARTESIAN_POINT('Origin',(17.,10.,2.));
#10763=CARTESIAN_POINT('',(16.835,10.,2.8));
#10764=CARTESIAN_POINT('',(16.835,10.,1.9));
#10765=CARTESIAN_POINT('Origin',(17.,10.,2.8));
#10766=CARTESIAN_POINT('Origin',(11.,10.,1.9));
#10767=CARTESIAN_POINT('',(10.835,10.,2.));
#10768=CARTESIAN_POINT('Origin',(11.,10.,2.));
#10769=CARTESIAN_POINT('',(10.835,10.,2.8));
#10770=CARTESIAN_POINT('',(10.835,10.,1.9));
#10771=CARTESIAN_POINT('Origin',(11.,10.,2.8));
#10772=CARTESIAN_POINT('Origin',(29.,10.,1.9));
#10773=CARTESIAN_POINT('',(28.835,10.,2.));
#10774=CARTESIAN_POINT('Origin',(29.,10.,2.));
#10775=CARTESIAN_POINT('',(28.835,10.,2.8));
#10776=CARTESIAN_POINT('',(28.835,10.,1.9));
#10777=CARTESIAN_POINT('Origin',(29.,10.,2.8));
#10778=CARTESIAN_POINT('Origin',(8.5,10.,1.9));
#10779=CARTESIAN_POINT('',(8.225,10.,2.));
#10780=CARTESIAN_POINT('Origin',(8.5,10.,2.));
#10781=CARTESIAN_POINT('',(8.225,10.,2.8));
#10782=CARTESIAN_POINT('',(8.225,10.,1.9));
#10783=CARTESIAN_POINT('Origin',(8.5,10.,2.8));
#10784=CARTESIAN_POINT('Origin',(31.5,10.,1.9));
#10785=CARTESIAN_POINT('',(31.225,10.,2.));
#10786=CARTESIAN_POINT('Origin',(31.5,10.,2.));
#10787=CARTESIAN_POINT('',(31.225,10.,2.8));
#10788=CARTESIAN_POINT('',(31.225,10.,1.9));
#10789=CARTESIAN_POINT('Origin',(31.5,10.,2.8));
#10790=CARTESIAN_POINT('Origin',(32.,12.5,2.));
#10791=CARTESIAN_POINT('',(32.,12.5,2.));
#10792=CARTESIAN_POINT('',(8.,12.5,2.));
#10793=CARTESIAN_POINT('',(32.,12.5,2.));
#10794=CARTESIAN_POINT('',(8.,12.5,2.8));
#10795=CARTESIAN_POINT('',(8.,12.5,2.));
#10796=CARTESIAN_POINT('',(32.,12.5,2.8));
#10797=CARTESIAN_POINT('',(32.,12.5,2.8));
#10798=CARTESIAN_POINT('',(32.,12.5,2.));
#10799=CARTESIAN_POINT('Origin',(32.,7.5,2.));
#10800=CARTESIAN_POINT('',(32.,7.5,2.));
#10801=CARTESIAN_POINT('',(32.,7.5,2.));
#10802=CARTESIAN_POINT('',(32.,7.5,2.8));
#10803=CARTESIAN_POINT('',(32.,7.5,2.8));
#10804=CARTESIAN_POINT('',(32.,7.5,2.));
#10805=CARTESIAN_POINT('Origin',(8.,7.5,2.));
#10806=CARTESIAN_POINT('',(8.,7.5,2.));
#10807=CARTESIAN_POINT('',(8.,7.5,2.));
#10808=CARTESIAN_POINT('',(8.,7.5,2.8));
#10809=CARTESIAN_POINT('',(8.,7.5,2.8));
#10810=CARTESIAN_POINT('',(8.,7.5,2.));
#10811=CARTESIAN_POINT('Origin',(8.,12.5,2.));
#10812=CARTESIAN_POINT('',(8.,12.5,2.));
#10813=CARTESIAN_POINT('',(8.,12.5,2.8));
#10814=CARTESIAN_POINT('Origin',(20.,10.,2.8));
#10815=CARTESIAN_POINT('Origin',(20.,10.,2.));
#10816=CARTESIAN_POINT('',(0.,0.,0.));
#10817=CARTESIAN_POINT('Origin',(1.,-10.,-0.9));
#10818=CARTESIAN_POINT('',(0.725,-10.,2.));
#10819=CARTESIAN_POINT('Origin',(1.,-10.,2.));
#10820=CARTESIAN_POINT('',(0.725,-10.,2.8));
#10821=CARTESIAN_POINT('',(0.725,-10.,-0.9));
#10822=CARTESIAN_POINT('Origin',(1.,-10.,2.8));
#10823=CARTESIAN_POINT('Origin',(1.,10.,-0.9));
#10824=CARTESIAN_POINT('',(0.725,10.,2.));
#10825=CARTESIAN_POINT('Origin',(1.,10.,2.));
#10826=CARTESIAN_POINT('',(0.725,10.,2.8));
#10827=CARTESIAN_POINT('',(0.725,10.,-0.9));
#10828=CARTESIAN_POINT('Origin',(1.,10.,2.8));
#10829=CARTESIAN_POINT('Origin',(2.,12.5,2.));
#10830=CARTESIAN_POINT('',(2.,12.5,2.));
#10831=CARTESIAN_POINT('',(0.,12.5,2.));
#10832=CARTESIAN_POINT('',(2.,12.5,2.));
#10833=CARTESIAN_POINT('',(0.,12.5,2.8));
#10834=CARTESIAN_POINT('',(0.,12.5,2.));
#10835=CARTESIAN_POINT('',(2.,12.5,2.8));
#10836=CARTESIAN_POINT('',(2.,12.5,2.8));
#10837=CARTESIAN_POINT('',(2.,12.5,2.));
#10838=CARTESIAN_POINT('Origin',(2.,-12.5,2.));
#10839=CARTESIAN_POINT('',(2.,-12.5,2.));
#10840=CARTESIAN_POINT('',(2.,-12.5,2.));
#10841=CARTESIAN_POINT('',(2.,-12.5,2.8));
#10842=CARTESIAN_POINT('',(2.,-12.5,2.8));
#10843=CARTESIAN_POINT('',(2.,-12.5,2.));
#10844=CARTESIAN_POINT('Origin',(0.,-12.5,2.));
#10845=CARTESIAN_POINT('',(0.,-12.5,2.));
#10846=CARTESIAN_POINT('',(0.,-12.5,2.));
#10847=CARTESIAN_POINT('',(0.,-12.5,2.8));
#10848=CARTESIAN_POINT('',(0.,-12.5,2.8));
#10849=CARTESIAN_POINT('',(0.,-12.5,2.));
#10850=CARTESIAN_POINT('Origin',(0.,12.5,2.));
#10851=CARTESIAN_POINT('',(0.,12.5,2.));
#10852=CARTESIAN_POINT('',(0.,12.5,2.8));
#10853=CARTESIAN_POINT('Origin',(1.,0.,2.8));
#10854=CARTESIAN_POINT('Origin',(1.,0.,2.));
#10855=CARTESIAN_POINT('',(0.,0.,0.));
#10856=CARTESIAN_POINT('Origin',(1.,-10.,-0.9));
#10857=CARTESIAN_POINT('',(0.725,-10.,-0.8));
#10858=CARTESIAN_POINT('Origin',(1.,-10.,-0.8));
#10859=CARTESIAN_POINT('',(0.725,-10.,0.));
#10860=CARTESIAN_POINT('',(0.725,-10.,-0.9));
#10861=CARTESIAN_POINT('Origin',(1.,-10.,0.));
#10862=CARTESIAN_POINT('Origin',(1.,10.,-0.9));
#10863=CARTESIAN_POINT('',(0.725,10.,-0.8));
#10864=CARTESIAN_POINT('Origin',(1.,10.,-0.8));
#10865=CARTESIAN_POINT('',(0.725,10.,0.));
#10866=CARTESIAN_POINT('',(0.725,10.,-0.9));
#10867=CARTESIAN_POINT('Origin',(1.,10.,0.));
#10868=CARTESIAN_POINT('Origin',(2.,12.5,-0.8));
#10869=CARTESIAN_POINT('',(2.,12.5,-0.8));
#10870=CARTESIAN_POINT('',(0.,12.5,-0.8));
#10871=CARTESIAN_POINT('',(2.,12.5,-0.8));
#10872=CARTESIAN_POINT('',(0.,12.5,0.));
#10873=CARTESIAN_POINT('',(0.,12.5,-0.8));
#10874=CARTESIAN_POINT('',(2.,12.5,0.));
#10875=CARTESIAN_POINT('',(2.,12.5,0.));
#10876=CARTESIAN_POINT('',(2.,12.5,-0.8));
#10877=CARTESIAN_POINT('Origin',(2.,-12.5,-0.8));
#10878=CARTESIAN_POINT('',(2.,-12.5,-0.8));
#10879=CARTESIAN_POINT('',(2.,-12.5,-0.8));
#10880=CARTESIAN_POINT('',(2.,-12.5,0.));
#10881=CARTESIAN_POINT('',(2.,-12.5,0.));
#10882=CARTESIAN_POINT('',(2.,-12.5,-0.8));
#10883=CARTESIAN_POINT('Origin',(0.,-12.5,-0.8));
#10884=CARTESIAN_POINT('',(0.,-12.5,-0.8));
#10885=CARTESIAN_POINT('',(0.,-12.5,-0.8));
#10886=CARTESIAN_POINT('',(0.,-12.5,0.));
#10887=CARTESIAN_POINT('',(0.,-12.5,0.));
#10888=CARTESIAN_POINT('',(0.,-12.5,-0.8));
#10889=CARTESIAN_POINT('Origin',(0.,12.5,-0.8));
#10890=CARTESIAN_POINT('',(0.,12.5,-0.8));
#10891=CARTESIAN_POINT('',(0.,12.5,0.));
#10892=CARTESIAN_POINT('Origin',(1.,0.,0.));
#10893=CARTESIAN_POINT('Origin',(1.,0.,-0.8));
#10894=CARTESIAN_POINT('',(0.,0.,0.));
#10895=CARTESIAN_POINT('Origin',(2.,-11.5,-1.1));
#10896=CARTESIAN_POINT('',(2.,-11.5,-1.1));
#10897=CARTESIAN_POINT('',(0.,-11.5,-1.1));
#10898=CARTESIAN_POINT('',(2.,-11.5,-1.1));
#10899=CARTESIAN_POINT('',(0.,-11.5,-0.8));
#10900=CARTESIAN_POINT('',(0.,-11.5,-1.1));
#10901=CARTESIAN_POINT('',(2.,-11.5,-0.8));
#10902=CARTESIAN_POINT('',(2.,-11.5,-0.8));
#10903=CARTESIAN_POINT('',(2.,-11.5,-1.1));
#10904=CARTESIAN_POINT('Origin',(2.,-12.5,-1.1));
#10905=CARTESIAN_POINT('',(2.,-12.5,-1.1));
#10906=CARTESIAN_POINT('',(2.,-12.5,-1.1));
#10907=CARTESIAN_POINT('',(2.,-12.5,-0.8));
#10908=CARTESIAN_POINT('',(2.,-12.5,-0.8));
#10909=CARTESIAN_POINT('',(2.,-12.5,-1.1));
#10910=CARTESIAN_POINT('Origin',(0.,-12.5,-1.1));
#10911=CARTESIAN_POINT('',(0.,-12.5,-1.1));
#10912=CARTESIAN_POINT('',(0.,-12.5,-1.1));
#10913=CARTESIAN_POINT('',(0.,-12.5,-0.8));
#10914=CARTESIAN_POINT('',(0.,-12.5,-0.8));
#10915=CARTESIAN_POINT('',(0.,-12.5,-1.1));
#10916=CARTESIAN_POINT('Origin',(0.,-11.5,-1.1));
#10917=CARTESIAN_POINT('',(0.,-11.5,-1.1));
#10918=CARTESIAN_POINT('',(0.,-11.5,-0.8));
#10919=CARTESIAN_POINT('Origin',(1.,-12.,-0.8));
#10920=CARTESIAN_POINT('Origin',(1.,-12.,-1.1));
#10921=CARTESIAN_POINT('',(0.,0.,0.));
#10922=CARTESIAN_POINT('Origin',(2.,12.5,-1.1));
#10923=CARTESIAN_POINT('',(2.,12.5,-1.1));
#10924=CARTESIAN_POINT('',(0.,12.5,-1.1));
#10925=CARTESIAN_POINT('',(2.,12.5,-1.1));
#10926=CARTESIAN_POINT('',(0.,12.5,-0.8));
#10927=CARTESIAN_POINT('',(0.,12.5,-1.1));
#10928=CARTESIAN_POINT('',(2.,12.5,-0.8));
#10929=CARTESIAN_POINT('',(2.,12.5,-0.8));
#10930=CARTESIAN_POINT('',(2.,12.5,-1.1));
#10931=CARTESIAN_POINT('Origin',(2.,11.5,-1.1));
#10932=CARTESIAN_POINT('',(2.,11.5,-1.1));
#10933=CARTESIAN_POINT('',(2.,11.5,-1.1));
#10934=CARTESIAN_POINT('',(2.,11.5,-0.8));
#10935=CARTESIAN_POINT('',(2.,11.5,-0.8));
#10936=CARTESIAN_POINT('',(2.,11.5,-1.1));
#10937=CARTESIAN_POINT('Origin',(0.,11.5,-1.1));
#10938=CARTESIAN_POINT('',(0.,11.5,-1.1));
#10939=CARTESIAN_POINT('',(0.,11.5,-1.1));
#10940=CARTESIAN_POINT('',(0.,11.5,-0.8));
#10941=CARTESIAN_POINT('',(0.,11.5,-0.8));
#10942=CARTESIAN_POINT('',(0.,11.5,-1.1));
#10943=CARTESIAN_POINT('Origin',(0.,12.5,-1.1));
#10944=CARTESIAN_POINT('',(0.,12.5,-1.1));
#10945=CARTESIAN_POINT('',(0.,12.5,-0.8));
#10946=CARTESIAN_POINT('Origin',(1.,12.,-0.8));
#10947=CARTESIAN_POINT('Origin',(1.,12.,-1.1));
#10948=CARTESIAN_POINT('',(0.,0.,0.));
#10949=CARTESIAN_POINT('Origin',(39.,-10.,-0.9));
#10950=CARTESIAN_POINT('',(38.725,-10.,2.));
#10951=CARTESIAN_POINT('Origin',(39.,-10.,2.));
#10952=CARTESIAN_POINT('',(38.725,-10.,2.8));
#10953=CARTESIAN_POINT('',(38.725,-10.,-0.9));
#10954=CARTESIAN_POINT('Origin',(39.,-10.,2.8));
#10955=CARTESIAN_POINT('Origin',(39.,10.,-0.9));
#10956=CARTESIAN_POINT('',(38.725,10.,2.));
#10957=CARTESIAN_POINT('Origin',(39.,10.,2.));
#10958=CARTESIAN_POINT('',(38.725,10.,2.8));
#10959=CARTESIAN_POINT('',(38.725,10.,-0.9));
#10960=CARTESIAN_POINT('Origin',(39.,10.,2.8));
#10961=CARTESIAN_POINT('Origin',(40.,12.5,2.));
#10962=CARTESIAN_POINT('',(40.,12.5,2.));
#10963=CARTESIAN_POINT('',(38.,12.5,2.));
#10964=CARTESIAN_POINT('',(40.,12.5,2.));
#10965=CARTESIAN_POINT('',(38.,12.5,2.8));
#10966=CARTESIAN_POINT('',(38.,12.5,2.));
#10967=CARTESIAN_POINT('',(40.,12.5,2.8));
#10968=CARTESIAN_POINT('',(40.,12.5,2.8));
#10969=CARTESIAN_POINT('',(40.,12.5,2.));
#10970=CARTESIAN_POINT('Origin',(40.,-12.5,2.));
#10971=CARTESIAN_POINT('',(40.,-12.5,2.));
#10972=CARTESIAN_POINT('',(40.,-12.5,2.));
#10973=CARTESIAN_POINT('',(40.,-12.5,2.8));
#10974=CARTESIAN_POINT('',(40.,-12.5,2.8));
#10975=CARTESIAN_POINT('',(40.,-12.5,2.));
#10976=CARTESIAN_POINT('Origin',(38.,-12.5,2.));
#10977=CARTESIAN_POINT('',(38.,-12.5,2.));
#10978=CARTESIAN_POINT('',(38.,-12.5,2.));
#10979=CARTESIAN_POINT('',(38.,-12.5,2.8));
#10980=CARTESIAN_POINT('',(38.,-12.5,2.8));
#10981=CARTESIAN_POINT('',(38.,-12.5,2.));
#10982=CARTESIAN_POINT('Origin',(38.,12.5,2.));
#10983=CARTESIAN_POINT('',(38.,12.5,2.));
#10984=CARTESIAN_POINT('',(38.,12.5,2.8));
#10985=CARTESIAN_POINT('Origin',(39.,0.,2.8));
#10986=CARTESIAN_POINT('Origin',(39.,0.,2.));
#10987=CARTESIAN_POINT('',(0.,0.,0.));
#10988=CARTESIAN_POINT('Origin',(39.,-10.,-0.9));
#10989=CARTESIAN_POINT('',(38.725,-10.,-0.8));
#10990=CARTESIAN_POINT('Origin',(39.,-10.,-0.8));
#10991=CARTESIAN_POINT('',(38.725,-10.,0.));
#10992=CARTESIAN_POINT('',(38.725,-10.,-0.9));
#10993=CARTESIAN_POINT('Origin',(39.,-10.,0.));
#10994=CARTESIAN_POINT('Origin',(39.,10.,-0.9));
#10995=CARTESIAN_POINT('',(38.725,10.,-0.8));
#10996=CARTESIAN_POINT('Origin',(39.,10.,-0.8));
#10997=CARTESIAN_POINT('',(38.725,10.,0.));
#10998=CARTESIAN_POINT('',(38.725,10.,-0.9));
#10999=CARTESIAN_POINT('Origin',(39.,10.,0.));
#11000=CARTESIAN_POINT('Origin',(40.,12.5,-0.8));
#11001=CARTESIAN_POINT('',(40.,12.5,-0.8));
#11002=CARTESIAN_POINT('',(38.,12.5,-0.8));
#11003=CARTESIAN_POINT('',(40.,12.5,-0.8));
#11004=CARTESIAN_POINT('',(38.,12.5,0.));
#11005=CARTESIAN_POINT('',(38.,12.5,-0.8));
#11006=CARTESIAN_POINT('',(40.,12.5,0.));
#11007=CARTESIAN_POINT('',(40.,12.5,0.));
#11008=CARTESIAN_POINT('',(40.,12.5,-0.8));
#11009=CARTESIAN_POINT('Origin',(40.,-12.5,-0.8));
#11010=CARTESIAN_POINT('',(40.,-12.5,-0.8));
#11011=CARTESIAN_POINT('',(40.,-12.5,-0.8));
#11012=CARTESIAN_POINT('',(40.,-12.5,0.));
#11013=CARTESIAN_POINT('',(40.,-12.5,0.));
#11014=CARTESIAN_POINT('',(40.,-12.5,-0.8));
#11015=CARTESIAN_POINT('Origin',(38.,-12.5,-0.8));
#11016=CARTESIAN_POINT('',(38.,-12.5,-0.8));
#11017=CARTESIAN_POINT('',(38.,-12.5,-0.8));
#11018=CARTESIAN_POINT('',(38.,-12.5,0.));
#11019=CARTESIAN_POINT('',(38.,-12.5,0.));
#11020=CARTESIAN_POINT('',(38.,-12.5,-0.8));
#11021=CARTESIAN_POINT('Origin',(38.,12.5,-0.8));
#11022=CARTESIAN_POINT('',(38.,12.5,-0.8));
#11023=CARTESIAN_POINT('',(38.,12.5,0.));
#11024=CARTESIAN_POINT('Origin',(39.,0.,0.));
#11025=CARTESIAN_POINT('Origin',(39.,0.,-0.8));
#11026=CARTESIAN_POINT('',(0.,0.,0.));
#11027=CARTESIAN_POINT('Origin',(40.,-11.5,-1.1));
#11028=CARTESIAN_POINT('',(40.,-11.5,-1.1));
#11029=CARTESIAN_POINT('',(38.,-11.5,-1.1));
#11030=CARTESIAN_POINT('',(40.,-11.5,-1.1));
#11031=CARTESIAN_POINT('',(38.,-11.5,-0.8));
#11032=CARTESIAN_POINT('',(38.,-11.5,-1.1));
#11033=CARTESIAN_POINT('',(40.,-11.5,-0.8));
#11034=CARTESIAN_POINT('',(40.,-11.5,-0.8));
#11035=CARTESIAN_POINT('',(40.,-11.5,-1.1));
#11036=CARTESIAN_POINT('Origin',(40.,-12.5,-1.1));
#11037=CARTESIAN_POINT('',(40.,-12.5,-1.1));
#11038=CARTESIAN_POINT('',(40.,-12.5,-1.1));
#11039=CARTESIAN_POINT('',(40.,-12.5,-0.8));
#11040=CARTESIAN_POINT('',(40.,-12.5,-0.8));
#11041=CARTESIAN_POINT('',(40.,-12.5,-1.1));
#11042=CARTESIAN_POINT('Origin',(38.,-12.5,-1.1));
#11043=CARTESIAN_POINT('',(38.,-12.5,-1.1));
#11044=CARTESIAN_POINT('',(38.,-12.5,-1.1));
#11045=CARTESIAN_POINT('',(38.,-12.5,-0.8));
#11046=CARTESIAN_POINT('',(38.,-12.5,-0.8));
#11047=CARTESIAN_POINT('',(38.,-12.5,-1.1));
#11048=CARTESIAN_POINT('Origin',(38.,-11.5,-1.1));
#11049=CARTESIAN_POINT('',(38.,-11.5,-1.1));
#11050=CARTESIAN_POINT('',(38.,-11.5,-0.8));
#11051=CARTESIAN_POINT('Origin',(39.,-12.,-0.8));
#11052=CARTESIAN_POINT('Origin',(39.,-12.,-1.1));
#11053=CARTESIAN_POINT('',(0.,0.,0.));
#11054=CARTESIAN_POINT('Origin',(40.,12.5,-1.1));
#11055=CARTESIAN_POINT('',(40.,12.5,-1.1));
#11056=CARTESIAN_POINT('',(38.,12.5,-1.1));
#11057=CARTESIAN_POINT('',(40.,12.5,-1.1));
#11058=CARTESIAN_POINT('',(38.,12.5,-0.8));
#11059=CARTESIAN_POINT('',(38.,12.5,-1.1));
#11060=CARTESIAN_POINT('',(40.,12.5,-0.8));
#11061=CARTESIAN_POINT('',(40.,12.5,-0.8));
#11062=CARTESIAN_POINT('',(40.,12.5,-1.1));
#11063=CARTESIAN_POINT('Origin',(40.,11.5,-1.1));
#11064=CARTESIAN_POINT('',(40.,11.5,-1.1));
#11065=CARTESIAN_POINT('',(40.,11.5,-1.1));
#11066=CARTESIAN_POINT('',(40.,11.5,-0.8));
#11067=CARTESIAN_POINT('',(40.,11.5,-0.8));
#11068=CARTESIAN_POINT('',(40.,11.5,-1.1));
#11069=CARTESIAN_POINT('Origin',(38.,11.5,-1.1));
#11070=CARTESIAN_POINT('',(38.,11.5,-1.1));
#11071=CARTESIAN_POINT('',(38.,11.5,-1.1));
#11072=CARTESIAN_POINT('',(38.,11.5,-0.8));
#11073=CARTESIAN_POINT('',(38.,11.5,-0.8));
#11074=CARTESIAN_POINT('',(38.,11.5,-1.1));
#11075=CARTESIAN_POINT('Origin',(38.,12.5,-1.1));
#11076=CARTESIAN_POINT('',(38.,12.5,-1.1));
#11077=CARTESIAN_POINT('',(38.,12.5,-0.8));
#11078=CARTESIAN_POINT('Origin',(39.,12.,-0.8));
#11079=CARTESIAN_POINT('Origin',(39.,12.,-1.1));
#11080=CARTESIAN_POINT('',(0.,0.,0.));
#11081=CARTESIAN_POINT('Origin',(7.5,-10.,2.9));
#11082=CARTESIAN_POINT('',(8.,-10.,2.9));
#11083=CARTESIAN_POINT('',(8.,-10.,6.2));
#11084=CARTESIAN_POINT('',(8.,-10.,2.9));
#11085=CARTESIAN_POINT('',(7.,-10.,6.2));
#11086=CARTESIAN_POINT('Origin',(7.5,-10.,6.2));
#11087=CARTESIAN_POINT('',(7.,-10.,2.9));
#11088=CARTESIAN_POINT('',(7.,-10.,2.9));
#11089=CARTESIAN_POINT('Origin',(7.5,-10.,2.9));
#11090=CARTESIAN_POINT('Origin',(7.5,-10.,2.9));
#11091=CARTESIAN_POINT('',(8.,-10.,2.9));
#11092=CARTESIAN_POINT('Origin',(7.5,-10.,2.9));
#11093=CARTESIAN_POINT('',(7.,-10.,2.9));
#11094=CARTESIAN_POINT('Origin',(7.5,-10.,6.2));
#11095=CARTESIAN_POINT('Origin',(7.5,-10.,2.9));
#11096=CARTESIAN_POINT('',(7.225,-10.,2.9));
#11097=CARTESIAN_POINT('Origin',(7.5,-10.,2.9));
#11098=CARTESIAN_POINT('Origin',(7.5,10.,2.9));
#11099=CARTESIAN_POINT('',(8.,10.,2.9));
#11100=CARTESIAN_POINT('',(8.,10.,6.2));
#11101=CARTESIAN_POINT('',(8.,10.,2.9));
#11102=CARTESIAN_POINT('',(7.,10.,6.2));
#11103=CARTESIAN_POINT('Origin',(7.5,10.,6.2));
#11104=CARTESIAN_POINT('',(7.,10.,2.9));
#11105=CARTESIAN_POINT('',(7.,10.,2.9));
#11106=CARTESIAN_POINT('Origin',(7.5,10.,2.9));
#11107=CARTESIAN_POINT('Origin',(7.5,10.,2.9));
#11108=CARTESIAN_POINT('',(8.,10.,2.9));
#11109=CARTESIAN_POINT('Origin',(7.5,10.,2.9));
#11110=CARTESIAN_POINT('',(7.,10.,2.9));
#11111=CARTESIAN_POINT('Origin',(7.5,10.,6.2));
#11112=CARTESIAN_POINT('Origin',(7.5,10.,2.9));
#11113=CARTESIAN_POINT('',(7.225,10.,2.9));
#11114=CARTESIAN_POINT('Origin',(7.5,10.,2.9));
#11115=CARTESIAN_POINT('Origin',(7.5,0.,6.2));
#11116=CARTESIAN_POINT('',(8.,12.5,6.2));
#11117=CARTESIAN_POINT('',(8.,-12.5,6.2));
#11118=CARTESIAN_POINT('',(7.,12.5,6.2));
#11119=CARTESIAN_POINT('',(8.,12.5,6.2));
#11120=CARTESIAN_POINT('',(7.,12.5,6.2));
#11121=CARTESIAN_POINT('Origin',(7.5,0.,6.2));
#11122=CARTESIAN_POINT('',(8.,-12.5,6.2));
#11123=CARTESIAN_POINT('',(7.,12.5,6.2));
#11124=CARTESIAN_POINT('Origin',(7.5,0.,6.2));
#11125=CARTESIAN_POINT('',(7.,-12.5,6.2));
#11126=CARTESIAN_POINT('',(7.,12.5,6.2));
#11127=CARTESIAN_POINT('',(8.,-12.5,6.2));
#11128=CARTESIAN_POINT('',(7.,-12.5,6.2));
#11129=CARTESIAN_POINT('',(8.,-12.5,6.2));
#11130=CARTESIAN_POINT('Origin',(7.5,-10.,1.9));
#11131=CARTESIAN_POINT('',(7.225,-10.,2.));
#11132=CARTESIAN_POINT('Origin',(7.5,-10.,2.));
#11133=CARTESIAN_POINT('',(7.225,-10.,1.9));
#11134=CARTESIAN_POINT('Origin',(7.5,10.,1.9));
#11135=CARTESIAN_POINT('',(7.225,10.,2.));
#11136=CARTESIAN_POINT('Origin',(7.5,10.,2.));
#11137=CARTESIAN_POINT('',(7.225,10.,1.9));
#11138=CARTESIAN_POINT('Origin',(8.,12.5,2.));
#11139=CARTESIAN_POINT('',(8.,12.5,2.));
#11140=CARTESIAN_POINT('',(7.,12.5,2.));
#11141=CARTESIAN_POINT('',(8.,12.5,2.));
#11142=CARTESIAN_POINT('',(7.,12.5,2.));
#11143=CARTESIAN_POINT('',(8.,12.5,2.));
#11144=CARTESIAN_POINT('Origin',(8.,-12.5,2.));
#11145=CARTESIAN_POINT('',(8.,-12.5,2.));
#11146=CARTESIAN_POINT('',(8.,-12.5,2.));
#11147=CARTESIAN_POINT('',(8.,-12.5,2.));
#11148=CARTESIAN_POINT('Origin',(7.,-12.5,2.));
#11149=CARTESIAN_POINT('',(7.,-12.5,2.));
#11150=CARTESIAN_POINT('',(7.,-12.5,2.));
#11151=CARTESIAN_POINT('',(7.,-12.5,2.));
#11152=CARTESIAN_POINT('Origin',(7.,12.5,2.));
#11153=CARTESIAN_POINT('',(7.,12.5,2.));
#11154=CARTESIAN_POINT('Origin',(7.5,0.,2.));
#11155=CARTESIAN_POINT('',(0.,0.,0.));
#11156=CARTESIAN_POINT('Origin',(8.2,12.5,5.2));
#11157=CARTESIAN_POINT('',(8.2,12.5,5.2));
#11158=CARTESIAN_POINT('',(8.,12.5,5.2));
#11159=CARTESIAN_POINT('',(8.2,12.5,5.2));
#11160=CARTESIAN_POINT('',(8.,12.5,6.2));
#11161=CARTESIAN_POINT('',(8.,12.5,5.2));
#11162=CARTESIAN_POINT('',(8.2,12.5,6.2));
#11163=CARTESIAN_POINT('',(8.2,12.5,6.2));
#11164=CARTESIAN_POINT('',(8.2,12.5,5.2));
#11165=CARTESIAN_POINT('Origin',(8.2,-12.5,5.2));
#11166=CARTESIAN_POINT('',(8.2,-12.5,5.2));
#11167=CARTESIAN_POINT('',(8.2,-12.5,5.2));
#11168=CARTESIAN_POINT('',(8.2,-12.5,6.2));
#11169=CARTESIAN_POINT('',(8.2,-12.5,6.2));
#11170=CARTESIAN_POINT('',(8.2,-12.5,5.2));
#11171=CARTESIAN_POINT('Origin',(8.,-12.5,5.2));
#11172=CARTESIAN_POINT('',(8.,-12.5,5.2));
#11173=CARTESIAN_POINT('',(8.,-12.5,5.2));
#11174=CARTESIAN_POINT('',(8.,-12.5,6.2));
#11175=CARTESIAN_POINT('',(8.,-12.5,6.2));
#11176=CARTESIAN_POINT('',(8.,-12.5,5.2));
#11177=CARTESIAN_POINT('Origin',(8.,12.5,5.2));
#11178=CARTESIAN_POINT('',(8.,12.5,5.2));
#11179=CARTESIAN_POINT('',(8.,12.5,6.2));
#11180=CARTESIAN_POINT('Origin',(8.1,0.,6.2));
#11181=CARTESIAN_POINT('Origin',(8.1,0.,5.2));
#11182=CARTESIAN_POINT('',(0.,0.,0.));
#11183=CARTESIAN_POINT('Origin',(32.5,-10.,2.9));
#11184=CARTESIAN_POINT('',(33.,-10.,2.9));
#11185=CARTESIAN_POINT('',(33.,-10.,6.2));
#11186=CARTESIAN_POINT('',(33.,-10.,2.9));
#11187=CARTESIAN_POINT('',(32.,-10.,6.2));
#11188=CARTESIAN_POINT('Origin',(32.5,-10.,6.2));
#11189=CARTESIAN_POINT('',(32.,-10.,2.9));
#11190=CARTESIAN_POINT('',(32.,-10.,2.9));
#11191=CARTESIAN_POINT('Origin',(32.5,-10.,2.9));
#11192=CARTESIAN_POINT('Origin',(32.5,-10.,2.9));
#11193=CARTESIAN_POINT('',(33.,-10.,2.9));
#11194=CARTESIAN_POINT('Origin',(32.5,-10.,2.9));
#11195=CARTESIAN_POINT('',(32.,-10.,2.9));
#11196=CARTESIAN_POINT('Origin',(32.5,-10.,6.2));
#11197=CARTESIAN_POINT('Origin',(32.5,-10.,2.9));
#11198=CARTESIAN_POINT('',(32.225,-10.,2.9));
#11199=CARTESIAN_POINT('Origin',(32.5,-10.,2.9));
#11200=CARTESIAN_POINT('Origin',(32.5,10.,2.9));
#11201=CARTESIAN_POINT('',(33.,10.,2.9));
#11202=CARTESIAN_POINT('',(33.,10.,6.2));
#11203=CARTESIAN_POINT('',(33.,10.,2.9));
#11204=CARTESIAN_POINT('',(32.,10.,6.2));
#11205=CARTESIAN_POINT('Origin',(32.5,10.,6.2));
#11206=CARTESIAN_POINT('',(32.,10.,2.9));
#11207=CARTESIAN_POINT('',(32.,10.,2.9));
#11208=CARTESIAN_POINT('Origin',(32.5,10.,2.9));
#11209=CARTESIAN_POINT('Origin',(32.5,10.,2.9));
#11210=CARTESIAN_POINT('',(33.,10.,2.9));
#11211=CARTESIAN_POINT('Origin',(32.5,10.,2.9));
#11212=CARTESIAN_POINT('',(32.,10.,2.9));
#11213=CARTESIAN_POINT('Origin',(32.5,10.,6.2));
#11214=CARTESIAN_POINT('Origin',(32.5,10.,2.9));
#11215=CARTESIAN_POINT('',(32.225,10.,2.9));
#11216=CARTESIAN_POINT('Origin',(32.5,10.,2.9));
#11217=CARTESIAN_POINT('Origin',(32.5,0.,6.2));
#11218=CARTESIAN_POINT('',(33.,12.5,6.2));
#11219=CARTESIAN_POINT('',(33.,-12.5,6.2));
#11220=CARTESIAN_POINT('',(32.,12.5,6.2));
#11221=CARTESIAN_POINT('',(33.,12.5,6.2));
#11222=CARTESIAN_POINT('',(32.,12.5,6.2));
#11223=CARTESIAN_POINT('Origin',(32.5,0.,6.2));
#11224=CARTESIAN_POINT('',(33.,-12.5,6.2));
#11225=CARTESIAN_POINT('',(32.,12.5,6.2));
#11226=CARTESIAN_POINT('Origin',(32.5,0.,6.2));
#11227=CARTESIAN_POINT('',(32.,-12.5,6.2));
#11228=CARTESIAN_POINT('',(32.,12.5,6.2));
#11229=CARTESIAN_POINT('',(33.,-12.5,6.2));
#11230=CARTESIAN_POINT('',(32.,-12.5,6.2));
#11231=CARTESIAN_POINT('',(33.,-12.5,6.2));
#11232=CARTESIAN_POINT('Origin',(32.5,-10.,1.9));
#11233=CARTESIAN_POINT('',(32.225,-10.,2.));
#11234=CARTESIAN_POINT('Origin',(32.5,-10.,2.));
#11235=CARTESIAN_POINT('',(32.225,-10.,1.9));
#11236=CARTESIAN_POINT('Origin',(32.5,10.,1.9));
#11237=CARTESIAN_POINT('',(32.225,10.,2.));
#11238=CARTESIAN_POINT('Origin',(32.5,10.,2.));
#11239=CARTESIAN_POINT('',(32.225,10.,1.9));
#11240=CARTESIAN_POINT('Origin',(33.,12.5,2.));
#11241=CARTESIAN_POINT('',(33.,12.5,2.));
#11242=CARTESIAN_POINT('',(32.,12.5,2.));
#11243=CARTESIAN_POINT('',(33.,12.5,2.));
#11244=CARTESIAN_POINT('',(32.,12.5,2.));
#11245=CARTESIAN_POINT('',(33.,12.5,2.));
#11246=CARTESIAN_POINT('Origin',(33.,-12.5,2.));
#11247=CARTESIAN_POINT('',(33.,-12.5,2.));
#11248=CARTESIAN_POINT('',(33.,-12.5,2.));
#11249=CARTESIAN_POINT('',(33.,-12.5,2.));
#11250=CARTESIAN_POINT('Origin',(32.,-12.5,2.));
#11251=CARTESIAN_POINT('',(32.,-12.5,2.));
#11252=CARTESIAN_POINT('',(32.,-12.5,2.));
#11253=CARTESIAN_POINT('',(32.,-12.5,2.));
#11254=CARTESIAN_POINT('Origin',(32.,12.5,2.));
#11255=CARTESIAN_POINT('',(32.,12.5,2.));
#11256=CARTESIAN_POINT('Origin',(32.5,0.,2.));
#11257=CARTESIAN_POINT('',(0.,0.,0.));
#11258=CARTESIAN_POINT('Origin',(32.,12.5,5.2));
#11259=CARTESIAN_POINT('',(32.,12.5,5.2));
#11260=CARTESIAN_POINT('',(31.8,12.5,5.2));
#11261=CARTESIAN_POINT('',(32.,12.5,5.2));
#11262=CARTESIAN_POINT('',(31.8,12.5,6.2));
#11263=CARTESIAN_POINT('',(31.8,12.5,5.2));
#11264=CARTESIAN_POINT('',(32.,12.5,6.2));
#11265=CARTESIAN_POINT('',(32.,12.5,6.2));
#11266=CARTESIAN_POINT('',(32.,12.5,5.2));
#11267=CARTESIAN_POINT('Origin',(32.,-12.5,5.2));
#11268=CARTESIAN_POINT('',(32.,-12.5,5.2));
#11269=CARTESIAN_POINT('',(32.,-12.5,5.2));
#11270=CARTESIAN_POINT('',(32.,-12.5,6.2));
#11271=CARTESIAN_POINT('',(32.,-12.5,6.2));
#11272=CARTESIAN_POINT('',(32.,-12.5,5.2));
#11273=CARTESIAN_POINT('Origin',(31.8,-12.5,5.2));
#11274=CARTESIAN_POINT('',(31.8,-12.5,5.2));
#11275=CARTESIAN_POINT('',(31.8,-12.5,5.2));
#11276=CARTESIAN_POINT('',(31.8,-12.5,6.2));
#11277=CARTESIAN_POINT('',(31.8,-12.5,6.2));
#11278=CARTESIAN_POINT('',(31.8,-12.5,5.2));
#11279=CARTESIAN_POINT('Origin',(31.8,12.5,5.2));
#11280=CARTESIAN_POINT('',(31.8,12.5,5.2));
#11281=CARTESIAN_POINT('',(31.8,12.5,6.2));
#11282=CARTESIAN_POINT('Origin',(31.9,0.,6.2));
#11283=CARTESIAN_POINT('Origin',(31.9,0.,5.2));
#11284=CARTESIAN_POINT('',(0.,0.,0.));
#11285=CARTESIAN_POINT('Origin',(-0.1,0.82,-0.3));
#11286=CARTESIAN_POINT('',(0.,0.82,-0.3));
#11287=CARTESIAN_POINT('',(0.,1.,-0.3));
#11288=CARTESIAN_POINT('',(0.,0.41,-0.3));
#11289=CARTESIAN_POINT('',(40.,0.82,-0.3));
#11290=CARTESIAN_POINT('',(-0.1,0.82,-0.3));
#11291=CARTESIAN_POINT('',(40.,1.,-0.3));
#11292=CARTESIAN_POINT('',(40.,0.41,-0.3));
#11293=CARTESIAN_POINT('',(-0.05,1.,-0.3));
#11294=CARTESIAN_POINT('Origin',(-0.1,0.82,-0.55));
#11295=CARTESIAN_POINT('',(0.,0.82,-0.55));
#11296=CARTESIAN_POINT('',(0.,0.82,-0.275));
#11297=CARTESIAN_POINT('',(40.,0.82,-0.55));
#11298=CARTESIAN_POINT('',(-0.1,0.82,-0.55));
#11299=CARTESIAN_POINT('',(40.,0.82,-0.275));
#11300=CARTESIAN_POINT('Origin',(-0.1,0.67,-0.55));
#11301=CARTESIAN_POINT('',(0.,0.67,-0.55));
#11302=CARTESIAN_POINT('',(0.,0.335,-0.55));
#11303=CARTESIAN_POINT('',(40.,0.67,-0.55));
#11304=CARTESIAN_POINT('',(-0.1,0.67,-0.55));
#11305=CARTESIAN_POINT('',(40.,0.335,-0.55));
#11306=CARTESIAN_POINT('Origin',(-0.1,0.42,-0.3));
#11307=CARTESIAN_POINT('',(0.,0.42,-0.3));
#11308=CARTESIAN_POINT('',(0.,0.24,-0.12));
#11309=CARTESIAN_POINT('',(40.,0.42,-0.3));
#11310=CARTESIAN_POINT('',(-0.1,0.42,-0.3));
#11311=CARTESIAN_POINT('',(40.,0.24,-0.12));
#11312=CARTESIAN_POINT('Origin',(-0.1,0.42,0.3));
#11313=CARTESIAN_POINT('',(0.,0.42,0.3));
#11314=CARTESIAN_POINT('',(0.,0.42,0.15));
#11315=CARTESIAN_POINT('',(40.,0.42,0.3));
#11316=CARTESIAN_POINT('',(-0.1,0.42,0.3));
#11317=CARTESIAN_POINT('',(40.,0.42,0.15));
#11318=CARTESIAN_POINT('Origin',(-0.1,0.67,0.55));
#11319=CARTESIAN_POINT('',(0.,0.67,0.55));
#11320=CARTESIAN_POINT('',(6.93889390390723E-18,0.365,0.245));
#11321=CARTESIAN_POINT('',(40.,0.67,0.55));
#11322=CARTESIAN_POINT('',(-0.1,0.67,0.55));
#11323=CARTESIAN_POINT('',(40.,0.365,0.245));
#11324=CARTESIAN_POINT('Origin',(-0.1,0.82,0.55));
#11325=CARTESIAN_POINT('',(0.,0.82,0.55));
#11326=CARTESIAN_POINT('',(0.,0.41,0.55));
#11327=CARTESIAN_POINT('',(40.,0.82,0.55));
#11328=CARTESIAN_POINT('',(-0.1,0.82,0.55));
#11329=CARTESIAN_POINT('',(40.,0.41,0.55));
#11330=CARTESIAN_POINT('Origin',(-0.1,0.82,0.3));
#11331=CARTESIAN_POINT('',(0.,0.82,0.3));
#11332=CARTESIAN_POINT('',(0.,0.82,0.15));
#11333=CARTESIAN_POINT('',(40.,0.82,0.3));
#11334=CARTESIAN_POINT('',(-0.1,0.82,0.3));
#11335=CARTESIAN_POINT('',(40.,0.82,0.15));
#11336=CARTESIAN_POINT('Origin',(-0.1,1.05,0.3));
#11337=CARTESIAN_POINT('',(0.,1.,0.3));
#11338=CARTESIAN_POINT('',(0.,0.525,0.3));
#11339=CARTESIAN_POINT('',(40.,1.,0.3));
#11340=CARTESIAN_POINT('',(-0.05,1.,0.3));
#11341=CARTESIAN_POINT('',(40.,0.525,0.3));
#11342=CARTESIAN_POINT('Origin',(-0.1,-0.3,-0.82));
#11343=CARTESIAN_POINT('',(0.,-0.3,-0.82));
#11344=CARTESIAN_POINT('',(0.,-0.3,-1.));
#11345=CARTESIAN_POINT('',(0.,-0.3,-0.41));
#11346=CARTESIAN_POINT('',(40.,-0.3,-0.82));
#11347=CARTESIAN_POINT('',(-0.1,-0.3,-0.82));
#11348=CARTESIAN_POINT('',(40.,-0.3,-1.));
#11349=CARTESIAN_POINT('',(40.,-0.3,-0.41));
#11350=CARTESIAN_POINT('',(-0.05,-0.3,-1.));
#11351=CARTESIAN_POINT('Origin',(-0.1,-0.55,-0.82));
#11352=CARTESIAN_POINT('',(0.,-0.55,-0.82));
#11353=CARTESIAN_POINT('',(0.,-0.275,-0.82));
#11354=CARTESIAN_POINT('',(40.,-0.55,-0.82));
#11355=CARTESIAN_POINT('',(-0.1,-0.55,-0.82));
#11356=CARTESIAN_POINT('',(40.,-0.275,-0.82));
#11357=CARTESIAN_POINT('Origin',(-0.1,-0.55,-0.67));
#11358=CARTESIAN_POINT('',(0.,-0.55,-0.67));
#11359=CARTESIAN_POINT('',(0.,-0.55,-0.335));
#11360=CARTESIAN_POINT('',(40.,-0.55,-0.67));
#11361=CARTESIAN_POINT('',(-0.1,-0.55,-0.67));
#11362=CARTESIAN_POINT('',(40.,-0.55,-0.335));
#11363=CARTESIAN_POINT('Origin',(-0.1,-0.3,-0.42));
#11364=CARTESIAN_POINT('',(0.,-0.3,-0.42));
#11365=CARTESIAN_POINT('',(0.,-0.12,-0.24));
#11366=CARTESIAN_POINT('',(40.,-0.3,-0.42));
#11367=CARTESIAN_POINT('',(-0.1,-0.3,-0.42));
#11368=CARTESIAN_POINT('',(40.,-0.12,-0.24));
#11369=CARTESIAN_POINT('Origin',(-0.1,0.3,-0.42));
#11370=CARTESIAN_POINT('',(0.,0.3,-0.42));
#11371=CARTESIAN_POINT('',(0.,0.15,-0.42));
#11372=CARTESIAN_POINT('',(40.,0.3,-0.42));
#11373=CARTESIAN_POINT('',(-0.1,0.3,-0.42));
#11374=CARTESIAN_POINT('',(40.,0.15,-0.42));
#11375=CARTESIAN_POINT('Origin',(-0.1,0.55,-0.67));
#11376=CARTESIAN_POINT('',(0.,0.55,-0.67));
#11377=CARTESIAN_POINT('',(0.,0.245,-0.365));
#11378=CARTESIAN_POINT('',(40.,0.55,-0.67));
#11379=CARTESIAN_POINT('',(-0.1,0.55,-0.67));
#11380=CARTESIAN_POINT('',(40.,0.245,-0.365));
#11381=CARTESIAN_POINT('Origin',(-0.1,0.55,-0.82));
#11382=CARTESIAN_POINT('',(0.,0.55,-0.82));
#11383=CARTESIAN_POINT('',(0.,0.55,-0.41));
#11384=CARTESIAN_POINT('',(40.,0.55,-0.82));
#11385=CARTESIAN_POINT('',(-0.1,0.55,-0.82));
#11386=CARTESIAN_POINT('',(40.,0.55,-0.41));
#11387=CARTESIAN_POINT('Origin',(-0.1,0.3,-0.82));
#11388=CARTESIAN_POINT('',(0.,0.3,-0.82));
#11389=CARTESIAN_POINT('',(0.,0.15,-0.82));
#11390=CARTESIAN_POINT('',(40.,0.3,-0.82));
#11391=CARTESIAN_POINT('',(-0.1,0.3,-0.82));
#11392=CARTESIAN_POINT('',(40.,0.15,-0.82));
#11393=CARTESIAN_POINT('Origin',(-0.1,0.3,-1.05));
#11394=CARTESIAN_POINT('',(0.,0.3,-1.));
#11395=CARTESIAN_POINT('',(0.,0.3,-0.525));
#11396=CARTESIAN_POINT('',(40.,0.3,-1.));
#11397=CARTESIAN_POINT('',(-0.05,0.3,-1.));
#11398=CARTESIAN_POINT('',(40.,0.3,-0.525));
#11399=CARTESIAN_POINT('Origin',(-0.1,-0.82,0.3));
#11400=CARTESIAN_POINT('',(0.,-0.82,0.3));
#11401=CARTESIAN_POINT('',(0.,-1.,0.3));
#11402=CARTESIAN_POINT('',(0.,-0.41,0.3));
#11403=CARTESIAN_POINT('',(40.,-0.82,0.3));
#11404=CARTESIAN_POINT('',(-0.1,-0.82,0.3));
#11405=CARTESIAN_POINT('',(40.,-1.,0.3));
#11406=CARTESIAN_POINT('',(40.,-0.41,0.3));
#11407=CARTESIAN_POINT('',(-0.05,-1.,0.3));
#11408=CARTESIAN_POINT('Origin',(-0.1,-0.82,0.55));
#11409=CARTESIAN_POINT('',(0.,-0.82,0.55));
#11410=CARTESIAN_POINT('',(0.,-0.82,0.275));
#11411=CARTESIAN_POINT('',(40.,-0.82,0.55));
#11412=CARTESIAN_POINT('',(-0.1,-0.82,0.55));
#11413=CARTESIAN_POINT('',(40.,-0.82,0.275));
#11414=CARTESIAN_POINT('Origin',(-0.1,-0.67,0.55));
#11415=CARTESIAN_POINT('',(0.,-0.67,0.55));
#11416=CARTESIAN_POINT('',(0.,-0.335,0.55));
#11417=CARTESIAN_POINT('',(40.,-0.67,0.55));
#11418=CARTESIAN_POINT('',(-0.1,-0.67,0.55));
#11419=CARTESIAN_POINT('',(40.,-0.335,0.55));
#11420=CARTESIAN_POINT('Origin',(-0.1,-0.42,0.3));
#11421=CARTESIAN_POINT('',(0.,-0.42,0.3));
#11422=CARTESIAN_POINT('',(-6.93889390390723E-18,-0.24,0.12));
#11423=CARTESIAN_POINT('',(40.,-0.42,0.3));
#11424=CARTESIAN_POINT('',(-0.1,-0.42,0.3));
#11425=CARTESIAN_POINT('',(40.,-0.24,0.12));
#11426=CARTESIAN_POINT('Origin',(-0.1,-0.42,-0.3));
#11427=CARTESIAN_POINT('',(0.,-0.42,-0.3));
#11428=CARTESIAN_POINT('',(0.,-0.42,-0.15));
#11429=CARTESIAN_POINT('',(40.,-0.42,-0.3));
#11430=CARTESIAN_POINT('',(-0.1,-0.42,-0.3));
#11431=CARTESIAN_POINT('',(40.,-0.42,-0.15));
#11432=CARTESIAN_POINT('Origin',(-0.1,-0.67,-0.55));
#11433=CARTESIAN_POINT('',(0.,-0.67,-0.55));
#11434=CARTESIAN_POINT('',(0.,-0.365,-0.245));
#11435=CARTESIAN_POINT('',(40.,-0.67,-0.55));
#11436=CARTESIAN_POINT('',(-0.1,-0.67,-0.55));
#11437=CARTESIAN_POINT('',(40.,-0.365,-0.245));
#11438=CARTESIAN_POINT('Origin',(-0.1,-0.82,-0.55));
#11439=CARTESIAN_POINT('',(0.,-0.82,-0.55));
#11440=CARTESIAN_POINT('',(0.,-0.41,-0.55));
#11441=CARTESIAN_POINT('',(40.,-0.82,-0.55));
#11442=CARTESIAN_POINT('',(-0.1,-0.82,-0.55));
#11443=CARTESIAN_POINT('',(40.,-0.41,-0.55));
#11444=CARTESIAN_POINT('Origin',(-0.1,-0.82,-0.3));
#11445=CARTESIAN_POINT('',(0.,-0.82,-0.3));
#11446=CARTESIAN_POINT('',(0.,-0.82,-0.15));
#11447=CARTESIAN_POINT('',(40.,-0.82,-0.3));
#11448=CARTESIAN_POINT('',(-0.1,-0.82,-0.3));
#11449=CARTESIAN_POINT('',(40.,-0.82,-0.15));
#11450=CARTESIAN_POINT('Origin',(-0.1,-1.05,-0.3));
#11451=CARTESIAN_POINT('',(0.,-1.,-0.3));
#11452=CARTESIAN_POINT('',(0.,-0.525,-0.3));
#11453=CARTESIAN_POINT('',(40.,-1.,-0.3));
#11454=CARTESIAN_POINT('',(-0.05,-1.,-0.3));
#11455=CARTESIAN_POINT('',(40.,-0.525,-0.3));
#11456=CARTESIAN_POINT('Origin',(-0.1,0.3,0.82));
#11457=CARTESIAN_POINT('',(0.,0.3,0.82));
#11458=CARTESIAN_POINT('',(0.,0.3,1.));
#11459=CARTESIAN_POINT('',(0.,0.3,0.41));
#11460=CARTESIAN_POINT('',(40.,0.3,0.82));
#11461=CARTESIAN_POINT('',(-0.1,0.3,0.82));
#11462=CARTESIAN_POINT('',(40.,0.3,1.));
#11463=CARTESIAN_POINT('',(40.,0.3,0.41));
#11464=CARTESIAN_POINT('',(-0.05,0.3,1.));
#11465=CARTESIAN_POINT('Origin',(-0.1,0.55,0.82));
#11466=CARTESIAN_POINT('',(0.,0.55,0.82));
#11467=CARTESIAN_POINT('',(0.,0.275,0.82));
#11468=CARTESIAN_POINT('',(40.,0.55,0.82));
#11469=CARTESIAN_POINT('',(-0.1,0.55,0.82));
#11470=CARTESIAN_POINT('',(40.,0.275,0.82));
#11471=CARTESIAN_POINT('Origin',(-0.1,0.55,0.67));
#11472=CARTESIAN_POINT('',(0.,0.55,0.67));
#11473=CARTESIAN_POINT('',(0.,0.55,0.335));
#11474=CARTESIAN_POINT('',(40.,0.55,0.67));
#11475=CARTESIAN_POINT('',(-0.1,0.55,0.67));
#11476=CARTESIAN_POINT('',(40.,0.55,0.335));
#11477=CARTESIAN_POINT('Origin',(-0.1,0.3,0.42));
#11478=CARTESIAN_POINT('',(0.,0.3,0.42));
#11479=CARTESIAN_POINT('',(6.93889390390723E-18,0.12,0.24));
#11480=CARTESIAN_POINT('',(40.,0.3,0.42));
#11481=CARTESIAN_POINT('',(-0.1,0.3,0.42));
#11482=CARTESIAN_POINT('',(40.,0.12,0.24));
#11483=CARTESIAN_POINT('Origin',(-0.1,-0.3,0.42));
#11484=CARTESIAN_POINT('',(0.,-0.3,0.42));
#11485=CARTESIAN_POINT('',(0.,-0.15,0.42));
#11486=CARTESIAN_POINT('',(40.,-0.3,0.42));
#11487=CARTESIAN_POINT('',(-0.1,-0.3,0.42));
#11488=CARTESIAN_POINT('',(40.,-0.15,0.42));
#11489=CARTESIAN_POINT('Origin',(-0.1,-0.55,0.67));
#11490=CARTESIAN_POINT('',(0.,-0.55,0.67));
#11491=CARTESIAN_POINT('',(6.93889390390723E-18,-0.245,0.365));
#11492=CARTESIAN_POINT('',(40.,-0.55,0.67));
#11493=CARTESIAN_POINT('',(-0.1,-0.55,0.67));
#11494=CARTESIAN_POINT('',(40.,-0.245,0.365));
#11495=CARTESIAN_POINT('Origin',(-0.1,-0.55,0.82));
#11496=CARTESIAN_POINT('',(0.,-0.55,0.82));
#11497=CARTESIAN_POINT('',(0.,-0.55,0.41));
#11498=CARTESIAN_POINT('',(40.,-0.55,0.82));
#11499=CARTESIAN_POINT('',(-0.1,-0.55,0.82));
#11500=CARTESIAN_POINT('',(40.,-0.55,0.41));
#11501=CARTESIAN_POINT('Origin',(-0.1,-0.3,0.82));
#11502=CARTESIAN_POINT('',(0.,-0.3,0.82));
#11503=CARTESIAN_POINT('',(0.,-0.15,0.82));
#11504=CARTESIAN_POINT('',(40.,-0.3,0.82));
#11505=CARTESIAN_POINT('',(-0.1,-0.3,0.82));
#11506=CARTESIAN_POINT('',(40.,-0.15,0.82));
#11507=CARTESIAN_POINT('Origin',(-0.1,-0.3,1.05));
#11508=CARTESIAN_POINT('',(0.,-0.3,1.));
#11509=CARTESIAN_POINT('',(0.,-0.3,0.525));
#11510=CARTESIAN_POINT('',(40.,-0.3,1.));
#11511=CARTESIAN_POINT('',(-0.05,-0.3,1.));
#11512=CARTESIAN_POINT('',(40.,-0.3,0.525));
#11513=CARTESIAN_POINT('Origin',(-0.1,0.,0.));
#11514=CARTESIAN_POINT('',(0.,-2.57175827820944E-17,0.21));
#11515=CARTESIAN_POINT('Origin',(0.,0.,0.));
#11516=CARTESIAN_POINT('',(40.,2.57175827820944E-17,0.21));
#11517=CARTESIAN_POINT('',(-0.1,-2.57175827820944E-17,0.21));
#11518=CARTESIAN_POINT('Origin',(40.,0.,0.));
#11519=CARTESIAN_POINT('Origin',(0.,1.,-1.));
#11520=CARTESIAN_POINT('',(0.,1.,1.));
#11521=CARTESIAN_POINT('',(0.,1.,-1.));
#11522=CARTESIAN_POINT('',(40.,1.,1.));
#11523=CARTESIAN_POINT('',(0.,1.,1.));
#11524=CARTESIAN_POINT('',(40.,1.,-1.));
#11525=CARTESIAN_POINT('Origin',(0.,1.,-1.));
#11526=CARTESIAN_POINT('',(40.,1.,-1.));
#11527=CARTESIAN_POINT('',(40.,1.,-1.));
#11528=CARTESIAN_POINT('',(0.,1.,-1.));
#11529=CARTESIAN_POINT('',(0.,1.,-1.));
#11530=CARTESIAN_POINT('',(0.,1.,-1.));
#11531=CARTESIAN_POINT('Origin',(0.,-1.,-1.));
#11532=CARTESIAN_POINT('',(0.,-1.,-1.));
#11533=CARTESIAN_POINT('',(40.,-1.,-1.));
#11534=CARTESIAN_POINT('Origin',(0.,-1.,-1.));
#11535=CARTESIAN_POINT('',(40.,-1.,-1.));
#11536=CARTESIAN_POINT('',(40.,-1.,-1.));
#11537=CARTESIAN_POINT('',(0.,-1.,-1.));
#11538=CARTESIAN_POINT('',(0.,-1.,-1.));
#11539=CARTESIAN_POINT('',(0.,-1.,-1.));
#11540=CARTESIAN_POINT('Origin',(0.,-1.,1.));
#11541=CARTESIAN_POINT('',(0.,-1.,1.));
#11542=CARTESIAN_POINT('',(40.,-1.,1.));
#11543=CARTESIAN_POINT('Origin',(0.,-1.,1.));
#11544=CARTESIAN_POINT('',(40.,-1.,1.));
#11545=CARTESIAN_POINT('',(40.,-1.,1.));
#11546=CARTESIAN_POINT('',(0.,-1.,1.));
#11547=CARTESIAN_POINT('',(0.,-1.,1.));
#11548=CARTESIAN_POINT('',(0.,-1.,1.));
#11549=CARTESIAN_POINT('Origin',(0.,1.,1.));
#11550=CARTESIAN_POINT('',(0.,1.,1.));
#11551=CARTESIAN_POINT('',(40.,1.,1.));
#11552=CARTESIAN_POINT('Origin',(0.,1.,1.));
#11553=CARTESIAN_POINT('',(40.,1.,1.));
#11554=CARTESIAN_POINT('',(0.,1.,1.));
#11555=CARTESIAN_POINT('Origin',(40.,0.,0.));
#11556=CARTESIAN_POINT('Origin',(0.,0.,0.));
#11557=CARTESIAN_POINT('',(0.,0.,0.));
#11558=CARTESIAN_POINT('Origin',(14.,0.,0.97));
#11559=CARTESIAN_POINT('',(13.625,-4.59242549680257E-17,0.97));
#11560=CARTESIAN_POINT('Origin',(14.,0.,0.97));
#11561=CARTESIAN_POINT('',(13.625,4.59242549680257E-17,1.5));
#11562=CARTESIAN_POINT('',(13.625,-4.59242549680257E-17,0.97));
#11563=CARTESIAN_POINT('Origin',(14.,0.,1.5));
#11564=CARTESIAN_POINT('Origin',(14.,0.,0.97));
#11565=CARTESIAN_POINT('',(13.775,-2.75545529808154E-17,0.97));
#11566=CARTESIAN_POINT('Origin',(14.,0.,0.97));
#11567=CARTESIAN_POINT('Origin',(8.,0.,0.97));
#11568=CARTESIAN_POINT('',(7.625,-4.59242549680257E-17,0.97));
#11569=CARTESIAN_POINT('Origin',(8.,0.,0.97));
#11570=CARTESIAN_POINT('',(7.625,4.59242549680257E-17,1.5));
#11571=CARTESIAN_POINT('',(7.625,-4.59242549680257E-17,0.97));
#11572=CARTESIAN_POINT('Origin',(8.,0.,1.5));
#11573=CARTESIAN_POINT('Origin',(8.,0.,0.97));
#11574=CARTESIAN_POINT('',(7.775,-2.75545529808154E-17,0.97));
#11575=CARTESIAN_POINT('Origin',(8.,0.,0.97));
#11576=CARTESIAN_POINT('Origin',(2.,0.,0.97));
#11577=CARTESIAN_POINT('',(1.625,-4.59242549680257E-17,0.97));
#11578=CARTESIAN_POINT('Origin',(2.,0.,0.97));
#11579=CARTESIAN_POINT('',(1.625,4.59242549680257E-17,1.5));
#11580=CARTESIAN_POINT('',(1.625,-4.59242549680257E-17,0.97));
#11581=CARTESIAN_POINT('Origin',(2.,0.,1.5));
#11582=CARTESIAN_POINT('Origin',(2.,0.,0.97));
#11583=CARTESIAN_POINT('',(1.775,-2.75545529808155E-17,0.97));
#11584=CARTESIAN_POINT('Origin',(2.,0.,0.97));
#11585=CARTESIAN_POINT('Origin',(20.,0.,0.97));
#11586=CARTESIAN_POINT('',(19.625,-4.59242549680257E-17,0.97));
#11587=CARTESIAN_POINT('Origin',(20.,0.,0.97));
#11588=CARTESIAN_POINT('',(19.625,4.59242549680257E-17,1.5));
#11589=CARTESIAN_POINT('',(19.625,-4.59242549680257E-17,0.97));
#11590=CARTESIAN_POINT('Origin',(20.,0.,1.5));
#11591=CARTESIAN_POINT('Origin',(20.,0.,0.97));
#11592=CARTESIAN_POINT('',(19.775,-2.75545529808156E-17,0.97));
#11593=CARTESIAN_POINT('Origin',(20.,0.,0.97));
#11594=CARTESIAN_POINT('Origin',(14.,0.,-0.1));
#11595=CARTESIAN_POINT('',(13.775,-2.75545529808154E-17,0.));
#11596=CARTESIAN_POINT('Origin',(14.,0.,0.));
#11597=CARTESIAN_POINT('',(13.775,-2.75545529808154E-17,-0.1));
#11598=CARTESIAN_POINT('Origin',(8.,0.,-0.1));
#11599=CARTESIAN_POINT('',(7.775,-2.75545529808154E-17,0.));
#11600=CARTESIAN_POINT('Origin',(8.,0.,0.));
#11601=CARTESIAN_POINT('',(7.775,-2.75545529808154E-17,-0.1));
#11602=CARTESIAN_POINT('Origin',(2.,0.,-0.1));
#11603=CARTESIAN_POINT('',(1.775,-2.75545529808155E-17,0.));
#11604=CARTESIAN_POINT('Origin',(2.,0.,0.));
#11605=CARTESIAN_POINT('',(1.775,-2.75545529808155E-17,-0.1));
#11606=CARTESIAN_POINT('Origin',(20.,0.,-0.1));
#11607=CARTESIAN_POINT('',(19.775,-2.75545529808156E-17,0.));
#11608=CARTESIAN_POINT('Origin',(20.,0.,0.));
#11609=CARTESIAN_POINT('',(19.775,-2.75545529808156E-17,-0.1));
#11610=CARTESIAN_POINT('Origin',(0.,-0.53,1.));
#11611=CARTESIAN_POINT('',(0.,-0.53,1.));
#11612=CARTESIAN_POINT('',(0.,-0.75,0.85));
#11613=CARTESIAN_POINT('',(0.,-0.53,1.));
#11614=CARTESIAN_POINT('',(22.,-0.75,0.85));
#11615=CARTESIAN_POINT('',(0.,-0.75,0.85));
#11616=CARTESIAN_POINT('',(22.,-0.53,1.));
#11617=CARTESIAN_POINT('',(22.,-0.53,1.));
#11618=CARTESIAN_POINT('',(0.,-0.53,1.));
#11619=CARTESIAN_POINT('Origin',(0.,-0.53,1.15));
#11620=CARTESIAN_POINT('',(0.,-0.53,1.15));
#11621=CARTESIAN_POINT('',(0.,-0.53,1.15));
#11622=CARTESIAN_POINT('',(22.,-0.53,1.15));
#11623=CARTESIAN_POINT('',(22.,-0.53,1.15));
#11624=CARTESIAN_POINT('',(0.,-0.53,1.15));
#11625=CARTESIAN_POINT('Origin',(0.,-0.75,1.3));
#11626=CARTESIAN_POINT('',(0.,-0.75,1.3));
#11627=CARTESIAN_POINT('',(0.,-0.75,1.3));
#11628=CARTESIAN_POINT('',(22.,-0.75,1.3));
#11629=CARTESIAN_POINT('',(22.,-0.75,1.3));
#11630=CARTESIAN_POINT('',(0.,-0.75,1.3));
#11631=CARTESIAN_POINT('Origin',(0.,-0.75,1.5));
#11632=CARTESIAN_POINT('',(0.,-0.75,1.5));
#11633=CARTESIAN_POINT('',(0.,-0.75,1.5));
#11634=CARTESIAN_POINT('',(22.,-0.75,1.5));
#11635=CARTESIAN_POINT('',(22.,-0.75,1.5));
#11636=CARTESIAN_POINT('',(0.,-0.75,1.5));
#11637=CARTESIAN_POINT('Origin',(0.,0.75,1.5));
#11638=CARTESIAN_POINT('',(0.,0.75,1.5));
#11639=CARTESIAN_POINT('',(0.,0.75,1.5));
#11640=CARTESIAN_POINT('',(22.,0.75,1.5));
#11641=CARTESIAN_POINT('',(22.,0.75,1.5));
#11642=CARTESIAN_POINT('',(0.,0.75,1.5));
#11643=CARTESIAN_POINT('Origin',(0.,0.75,1.3));
#11644=CARTESIAN_POINT('',(0.,0.75,1.3));
#11645=CARTESIAN_POINT('',(0.,0.75,1.3));
#11646=CARTESIAN_POINT('',(22.,0.75,1.3));
#11647=CARTESIAN_POINT('',(22.,0.75,1.3));
#11648=CARTESIAN_POINT('',(0.,0.75,1.3));
#11649=CARTESIAN_POINT('Origin',(0.,0.53,1.15));
#11650=CARTESIAN_POINT('',(0.,0.53,1.15));
#11651=CARTESIAN_POINT('',(0.,0.53,1.15));
#11652=CARTESIAN_POINT('',(22.,0.53,1.15));
#11653=CARTESIAN_POINT('',(22.,0.53,1.15));
#11654=CARTESIAN_POINT('',(0.,0.53,1.15));
#11655=CARTESIAN_POINT('Origin',(0.,0.53,1.));
#11656=CARTESIAN_POINT('',(0.,0.53,1.));
#11657=CARTESIAN_POINT('',(0.,0.53,1.));
#11658=CARTESIAN_POINT('',(22.,0.53,1.));
#11659=CARTESIAN_POINT('',(22.,0.53,1.));
#11660=CARTESIAN_POINT('',(0.,0.53,1.));
#11661=CARTESIAN_POINT('Origin',(0.,0.75,0.85));
#11662=CARTESIAN_POINT('',(0.,0.75,0.85));
#11663=CARTESIAN_POINT('',(0.,0.75,0.85));
#11664=CARTESIAN_POINT('',(22.,0.75,0.85));
#11665=CARTESIAN_POINT('',(22.,0.75,0.85));
#11666=CARTESIAN_POINT('',(0.,0.75,0.85));
#11667=CARTESIAN_POINT('Origin',(0.,0.75,0.));
#11668=CARTESIAN_POINT('',(0.,0.75,0.));
#11669=CARTESIAN_POINT('',(0.,0.75,0.));
#11670=CARTESIAN_POINT('',(22.,0.75,0.));
#11671=CARTESIAN_POINT('',(22.,0.75,0.));
#11672=CARTESIAN_POINT('',(0.,0.75,0.));
#11673=CARTESIAN_POINT('Origin',(0.,-0.75,0.));
#11674=CARTESIAN_POINT('',(0.,-0.75,0.));
#11675=CARTESIAN_POINT('',(0.,-0.75,0.));
#11676=CARTESIAN_POINT('',(22.,-0.75,0.));
#11677=CARTESIAN_POINT('',(22.,-0.75,0.));
#11678=CARTESIAN_POINT('',(0.,-0.75,0.));
#11679=CARTESIAN_POINT('Origin',(0.,-0.75,0.85));
#11680=CARTESIAN_POINT('',(0.,-0.75,0.85));
#11681=CARTESIAN_POINT('',(22.,-0.75,0.85));
#11682=CARTESIAN_POINT('Origin',(22.,0.,0.75));
#11683=CARTESIAN_POINT('Origin',(0.,0.,0.75));
#11684=CARTESIAN_POINT('',(0.,0.,0.));
#11685=CARTESIAN_POINT('Origin',(0.3,0.4,0.));
#11686=CARTESIAN_POINT('',(-0.3,0.4,-3.67394039744206E-17));
#11687=CARTESIAN_POINT('Origin',(0.,0.4,0.));
#11688=CARTESIAN_POINT('Origin',(0.,0.375,0.));
#11689=CARTESIAN_POINT('',(-0.35,0.35,-4.28626379701573E-17));
#11690=CARTESIAN_POINT('Origin',(0.,0.35,0.));
#11691=CARTESIAN_POINT('',(-0.325,0.375,-3.9801020972289E-17));
#11692=CARTESIAN_POINT('Origin',(0.,0.19,0.));
#11693=CARTESIAN_POINT('',(-0.35,0.03,-4.28626379701574E-17));
#11694=CARTESIAN_POINT('Origin',(0.,0.03,0.));
#11695=CARTESIAN_POINT('',(-0.35,0.19,-4.28626379701574E-17));
#11696=CARTESIAN_POINT('Origin',(0.,0.0149999999999999,0.));
#11697=CARTESIAN_POINT('',(-0.32,-3.29597460435593E-17,-3.91886975727153E-17));
#11698=CARTESIAN_POINT('Origin',(0.,0.,0.));
#11699=CARTESIAN_POINT('',(-0.335,0.0149999999999999,-4.10256677714363E-17));
#11700=CARTESIAN_POINT('Origin',(0.22,0.,0.));
#11701=CARTESIAN_POINT('',(-0.22,-6.93889390390723E-18,-2.69422295812418E-17));
#11702=CARTESIAN_POINT('Origin',(0.,0.,0.));
#11703=CARTESIAN_POINT('Origin',(0.,-0.02,0.));
#11704=CARTESIAN_POINT('',(-0.1954,-0.0492,2.39295984553393E-17));
#11705=CARTESIAN_POINT('Origin',(0.,-0.0492,0.));
#11706=CARTESIAN_POINT('',(-0.21,-0.02,-2.57175827820944E-17));
#11707=CARTESIAN_POINT('Origin',(0.,-0.8,0.));
#11708=CARTESIAN_POINT('',(-0.1954,-1.5646,2.39295984553393E-17));
#11709=CARTESIAN_POINT('Origin',(0.,-1.5646,0.));
#11710=CARTESIAN_POINT('',(-0.1954,-0.8,-2.39295984553393E-17));
#11711=CARTESIAN_POINT('Origin',(0.,-1.58,0.));
#11712=CARTESIAN_POINT('',(-0.16,-1.6,-1.95943487863577E-17));
#11713=CARTESIAN_POINT('Origin',(0.,-1.6,0.));
#11714=CARTESIAN_POINT('',(-0.18,-1.58,-2.20436423846524E-17));
#11715=CARTESIAN_POINT('Origin',(0.,-1.6,0.));
#11716=CARTESIAN_POINT('Origin',(0.0866025403784439,-0.4,-0.15));
#11717=CARTESIAN_POINT('',(0.173205080756888,-0.4,0.));
#11718=CARTESIAN_POINT('',(0.0866025403784439,-0.4,-0.15));
#11719=CARTESIAN_POINT('',(0.173205080756888,-0.4,0.));
#11720=CARTESIAN_POINT('',(0.0866025403784439,-0.64,-0.15));
#11721=CARTESIAN_POINT('',(0.0866025403784439,-0.4,-0.15));
#11722=CARTESIAN_POINT('',(0.173205080756888,-0.64,0.));
#11723=CARTESIAN_POINT('',(0.173205080756888,-0.64,0.));
#11724=CARTESIAN_POINT('',(0.173205080756888,-0.4,0.));
#11725=CARTESIAN_POINT('Origin',(-0.0866025403784438,-0.4,-0.15));
#11726=CARTESIAN_POINT('',(-0.0866025403784438,-0.4,-0.15));
#11727=CARTESIAN_POINT('',(0.0866025403784439,-0.4,-0.15));
#11728=CARTESIAN_POINT('',(-0.0866025403784438,-0.64,-0.15));
#11729=CARTESIAN_POINT('',(-0.0866025403784438,-0.4,-0.15));
#11730=CARTESIAN_POINT('',(0.0866025403784439,-0.64,-0.15));
#11731=CARTESIAN_POINT('Origin',(-0.173205080756888,-0.4,-2.77555756156289E-17));
#11732=CARTESIAN_POINT('',(-0.173205080756888,-0.4,-2.12115047744981E-17));
#11733=CARTESIAN_POINT('',(-0.0866025403784438,-0.4,-0.15));
#11734=CARTESIAN_POINT('',(-0.173205080756888,-0.64,-2.77555756156289E-17));
#11735=CARTESIAN_POINT('',(-0.173205080756888,-0.4,-2.12115047744981E-17));
#11736=CARTESIAN_POINT('',(-0.0866025403784438,-0.64,-0.15));
#11737=CARTESIAN_POINT('Origin',(-0.0866025403784439,-0.4,0.15));
#11738=CARTESIAN_POINT('',(-0.0866025403784439,-0.4,0.15));
#11739=CARTESIAN_POINT('',(-0.173205080756888,-0.4,-2.12115047744981E-17));
#11740=CARTESIAN_POINT('',(-0.0866025403784439,-0.64,0.15));
#11741=CARTESIAN_POINT('',(-0.0866025403784439,-0.4,0.15));
#11742=CARTESIAN_POINT('',(-0.173205080756888,-0.64,-2.12115047744981E-17));
#11743=CARTESIAN_POINT('Origin',(0.0866025403784439,-0.4,0.15));
#11744=CARTESIAN_POINT('',(0.0866025403784439,-0.4,0.15));
#11745=CARTESIAN_POINT('',(-0.0866025403784439,-0.4,0.15));
#11746=CARTESIAN_POINT('',(0.0866025403784439,-0.64,0.15));
#11747=CARTESIAN_POINT('',(0.0866025403784439,-0.4,0.15));
#11748=CARTESIAN_POINT('',(-0.0866025403784439,-0.64,0.15));
#11749=CARTESIAN_POINT('Origin',(0.173205080756888,-0.4,0.));
#11750=CARTESIAN_POINT('',(0.0866025403784439,-0.4,0.15));
#11751=CARTESIAN_POINT('',(0.0866025403784439,-0.64,0.15));
#11752=CARTESIAN_POINT('Origin',(0.,-0.4,-2.77555756156289E-17));
#11753=CARTESIAN_POINT('Origin',(0.,-0.64,-2.77555756156289E-17));
#11754=CARTESIAN_POINT('',(0.,0.,0.));
#11755=CARTESIAN_POINT('Origin',(0.,0.395,0.25));
#11756=CARTESIAN_POINT('',(-0.5,0.3,0.25));
#11757=CARTESIAN_POINT('',(0.5,0.3,0.25));
#11758=CARTESIAN_POINT('',(0.25,0.3,0.25));
#11759=CARTESIAN_POINT('',(-0.5,0.5,0.25));
#11760=CARTESIAN_POINT('',(-0.5,0.5,0.25));
#11761=CARTESIAN_POINT('',(0.5,0.5,0.25));
#11762=CARTESIAN_POINT('',(0.5,0.5,0.25));
#11763=CARTESIAN_POINT('',(0.5,0.29,0.25));
#11764=CARTESIAN_POINT('Origin',(0.5,0.5,0.25));
#11765=CARTESIAN_POINT('',(-0.5,0.5,0.4));
#11766=CARTESIAN_POINT('',(-0.5,0.5,0.25));
#11767=CARTESIAN_POINT('',(0.5,0.5,0.4));
#11768=CARTESIAN_POINT('',(0.5,0.5,0.4));
#11769=CARTESIAN_POINT('',(0.5,0.5,0.25));
#11770=CARTESIAN_POINT('Origin',(0.,0.,0.4));
#11771=CARTESIAN_POINT('',(-0.5,-0.5,0.4));
#11772=CARTESIAN_POINT('',(-0.5,0.5,0.4));
#11773=CARTESIAN_POINT('',(0.5,-0.5,0.4));
#11774=CARTESIAN_POINT('',(-0.5,-0.5,0.4));
#11775=CARTESIAN_POINT('',(0.5,-0.3,0.4));
#11776=CARTESIAN_POINT('',(-0.2117,2.59257727379495E-17,0.4));
#11777=CARTESIAN_POINT('Origin',(0.,0.,0.4));
#11778=CARTESIAN_POINT('Origin',(-0.5,0.3,0.));
#11779=CARTESIAN_POINT('',(-0.5,0.3,0.15));
#11780=CARTESIAN_POINT('',(-0.5,0.3,0.));
#11781=CARTESIAN_POINT('',(-0.5,0.15,0.));
#11782=CARTESIAN_POINT('',(-0.5,0.225,0.075));
#11783=CARTESIAN_POINT('',(-0.5,-0.15,0.));
#11784=CARTESIAN_POINT('',(-0.5,0.3,0.));
#11785=CARTESIAN_POINT('',(-0.5,-0.3,0.15));
#11786=CARTESIAN_POINT('',(-0.5,-0.075,-0.075));
#11787=CARTESIAN_POINT('',(-0.5,-0.3,0.25));
#11788=CARTESIAN_POINT('',(-0.5,-0.3,0.));
#11789=CARTESIAN_POINT('',(-0.5,-0.5,0.25));
#11790=CARTESIAN_POINT('',(-0.5,-0.29,0.25));
#11791=CARTESIAN_POINT('',(-0.5,-0.5,0.25));
#11792=CARTESIAN_POINT('Origin',(-0.5,-0.5,0.25));
#11793=CARTESIAN_POINT('',(0.5,-0.5,0.25));
#11794=CARTESIAN_POINT('',(-0.5,-0.5,0.25));
#11795=CARTESIAN_POINT('',(0.5,-0.5,0.25));
#11796=CARTESIAN_POINT('Origin',(0.,-0.395,0.25));
#11797=CARTESIAN_POINT('',(0.5,-0.3,0.25));
#11798=CARTESIAN_POINT('',(-0.25,-0.3,0.25));
#11799=CARTESIAN_POINT('',(0.5,-0.5,0.25));
#11800=CARTESIAN_POINT('Origin',(0.5,-0.3,0.));
#11801=CARTESIAN_POINT('',(0.5,-0.3,0.15));
#11802=CARTESIAN_POINT('',(0.5,-0.3,0.));
#11803=CARTESIAN_POINT('',(0.5,-0.15,0.));
#11804=CARTESIAN_POINT('',(0.5,-0.225,0.075));
#11805=CARTESIAN_POINT('',(0.5,0.15,0.));
#11806=CARTESIAN_POINT('',(0.5,-0.3,0.));
#11807=CARTESIAN_POINT('',(0.5,0.3,0.15));
#11808=CARTESIAN_POINT('',(0.5,0.075,-0.075));
#11809=CARTESIAN_POINT('',(0.5,0.3,0.));
#11810=CARTESIAN_POINT('Origin',(-0.5,-0.3,0.));
#11811=CARTESIAN_POINT('',(-0.25,-0.3,0.15));
#11812=CARTESIAN_POINT('Origin',(-0.25,-0.225,0.075));
#11813=CARTESIAN_POINT('',(-0.149388386429468,-0.15,0.));
#11814=CARTESIAN_POINT('',(-0.25,-0.15,0.));
#11815=CARTESIAN_POINT('',(0.149388386429468,-0.15,0.));
#11816=CARTESIAN_POINT('Origin',(0.,0.,-0.15));
#11817=CARTESIAN_POINT('',(-0.25,-0.15,0.));
#11818=CARTESIAN_POINT('Origin',(0.,0.,-0.1));
#11819=CARTESIAN_POINT('',(-0.2117,-2.59257727379495E-17,0.));
#11820=CARTESIAN_POINT('Origin',(0.,0.,0.));
#11821=CARTESIAN_POINT('',(-0.2117,-2.59257727379495E-17,-0.1));
#11822=CARTESIAN_POINT('',(-0.149388386429468,0.15,0.));
#11823=CARTESIAN_POINT('Origin',(0.,0.,0.));
#11824=CARTESIAN_POINT('',(0.149388386429468,0.15,0.));
#11825=CARTESIAN_POINT('Origin',(0.,0.,-0.15));
#11826=CARTESIAN_POINT('Origin',(0.,0.,0.));
#11827=CARTESIAN_POINT('Origin',(0.,0.,0.));
#11828=CARTESIAN_POINT('',(0.25,0.15,0.));
#11829=CARTESIAN_POINT('Origin',(0.,0.,0.));
#11830=CARTESIAN_POINT('',(0.25,0.15,0.));
#11831=CARTESIAN_POINT('Origin',(0.25,0.225,0.075));
#11832=CARTESIAN_POINT('',(0.25,0.3,0.15));
#11833=CARTESIAN_POINT('Origin',(0.5,0.3,0.));
#11834=CARTESIAN_POINT('',(0.,0.,0.));
#11835=CARTESIAN_POINT('Origin',(0.115470053837925,-0.5,-0.2));
#11836=CARTESIAN_POINT('',(0.23094010767585,-0.5,0.));
#11837=CARTESIAN_POINT('',(0.115470053837925,-0.5,-0.2));
#11838=CARTESIAN_POINT('',(0.23094010767585,-0.5,0.));
#11839=CARTESIAN_POINT('',(0.115470053837925,-0.8,-0.2));
#11840=CARTESIAN_POINT('',(0.115470053837925,-0.5,-0.2));
#11841=CARTESIAN_POINT('',(0.23094010767585,-0.8,0.));
#11842=CARTESIAN_POINT('',(0.23094010767585,-0.8,0.));
#11843=CARTESIAN_POINT('',(0.23094010767585,-0.5,0.));
#11844=CARTESIAN_POINT('Origin',(-0.115470053837925,-0.5,-0.2));
#11845=CARTESIAN_POINT('',(-0.115470053837925,-0.5,-0.2));
#11846=CARTESIAN_POINT('',(0.115470053837925,-0.5,-0.2));
#11847=CARTESIAN_POINT('',(-0.115470053837925,-0.8,-0.2));
#11848=CARTESIAN_POINT('',(-0.115470053837925,-0.5,-0.2));
#11849=CARTESIAN_POINT('',(0.115470053837925,-0.8,-0.2));
#11850=CARTESIAN_POINT('Origin',(-0.23094010767585,-0.5,-2.77555756156289E-17));
#11851=CARTESIAN_POINT('',(-0.23094010767585,-0.5,-2.82820063659975E-17));
#11852=CARTESIAN_POINT('',(-0.115470053837925,-0.5,-0.2));
#11853=CARTESIAN_POINT('',(-0.23094010767585,-0.8,-2.77555756156289E-17));
#11854=CARTESIAN_POINT('',(-0.23094010767585,-0.5,-2.82820063659975E-17));
#11855=CARTESIAN_POINT('',(-0.115470053837925,-0.8,-0.2));
#11856=CARTESIAN_POINT('Origin',(-0.115470053837925,-0.5,0.2));
#11857=CARTESIAN_POINT('',(-0.115470053837925,-0.5,0.2));
#11858=CARTESIAN_POINT('',(-0.23094010767585,-0.5,-2.82820063659975E-17));
#11859=CARTESIAN_POINT('',(-0.115470053837925,-0.8,0.2));
#11860=CARTESIAN_POINT('',(-0.115470053837925,-0.5,0.2));
#11861=CARTESIAN_POINT('',(-0.23094010767585,-0.8,-2.82820063659975E-17));
#11862=CARTESIAN_POINT('Origin',(0.115470053837925,-0.5,0.2));
#11863=CARTESIAN_POINT('',(0.115470053837925,-0.5,0.2));
#11864=CARTESIAN_POINT('',(-0.115470053837925,-0.5,0.2));
#11865=CARTESIAN_POINT('',(0.115470053837925,-0.8,0.2));
#11866=CARTESIAN_POINT('',(0.115470053837925,-0.5,0.2));
#11867=CARTESIAN_POINT('',(-0.115470053837925,-0.8,0.2));
#11868=CARTESIAN_POINT('Origin',(0.23094010767585,-0.5,0.));
#11869=CARTESIAN_POINT('',(0.115470053837925,-0.5,0.2));
#11870=CARTESIAN_POINT('',(0.115470053837925,-0.8,0.2));
#11871=CARTESIAN_POINT('Origin',(0.,-0.5,0.));
#11872=CARTESIAN_POINT('Origin',(0.,-0.8,0.));
#11873=CARTESIAN_POINT('Origin',(0.,-1.4,0.));
#11874=CARTESIAN_POINT('',(-0.24505,-1.4,3.00099698131059E-17));
#11875=CARTESIAN_POINT('Origin',(0.,-1.4,0.));
#11876=CARTESIAN_POINT('Origin',(0.375,0.5,0.));
#11877=CARTESIAN_POINT('',(-0.375,0.5,-4.59242549680257E-17));
#11878=CARTESIAN_POINT('Origin',(0.,0.5,0.));
#11879=CARTESIAN_POINT('Origin',(0.,0.475,0.));
#11880=CARTESIAN_POINT('',(-0.425,0.45,-5.20474889637625E-17));
#11881=CARTESIAN_POINT('Origin',(0.,0.45,0.));
#11882=CARTESIAN_POINT('',(-0.4,0.475,-4.89858719658941E-17));
#11883=CARTESIAN_POINT('Origin',(0.,0.24,0.));
#11884=CARTESIAN_POINT('',(-0.425,0.0299999999999998,-5.20474889637625E-17));
#11885=CARTESIAN_POINT('Origin',(0.,0.0299999999999998,0.));
#11886=CARTESIAN_POINT('',(-0.425,0.24,-5.20474889637625E-17));
#11887=CARTESIAN_POINT('Origin',(0.,0.0150000000000001,0.));
#11888=CARTESIAN_POINT('',(-0.395,4.85722573273506E-17,-4.83735485663204E-17));
#11889=CARTESIAN_POINT('Origin',(0.,0.,0.));
#11890=CARTESIAN_POINT('',(-0.41,0.0150000000000001,-5.02105187650415E-17));
#11891=CARTESIAN_POINT('Origin',(0.27,0.,0.));
#11892=CARTESIAN_POINT('',(-0.27,0.,-3.30654635769785E-17));
#11893=CARTESIAN_POINT('Origin',(0.,0.,0.));
#11894=CARTESIAN_POINT('Origin',(0.,-0.02,0.));
#11895=CARTESIAN_POINT('',(-0.24505,-0.0498999999999999,3.00099698131059E-17));
#11896=CARTESIAN_POINT('Origin',(0.,-0.0498999999999999,0.));
#11897=CARTESIAN_POINT('',(-0.26,-0.02,-3.18408167778312E-17));
#11898=CARTESIAN_POINT('Origin',(0.,-0.995,0.));
#11899=CARTESIAN_POINT('',(-0.24505,-0.995,-3.00099698131059E-17));
#11900=CARTESIAN_POINT('',(0.,0.,0.));
#11901=CARTESIAN_POINT('',(0.,0.,0.));
#11902=CARTESIAN_POINT('Origin',(19.5,12.5,5.1));
#11903=CARTESIAN_POINT('',(19.335,12.5,5.2));
#11904=CARTESIAN_POINT('Origin',(19.5,12.5,5.2));
#11905=CARTESIAN_POINT('',(19.335,12.5,6.4));
#11906=CARTESIAN_POINT('',(19.335,12.5,5.1));
#11907=CARTESIAN_POINT('Origin',(19.5,12.5,6.4));
#11908=CARTESIAN_POINT('Origin',(20.5,12.5,5.1));
#11909=CARTESIAN_POINT('',(20.335,12.5,5.2));
#11910=CARTESIAN_POINT('Origin',(20.5,12.5,5.2));
#11911=CARTESIAN_POINT('',(20.335,12.5,6.4));
#11912=CARTESIAN_POINT('',(20.335,12.5,5.1));
#11913=CARTESIAN_POINT('Origin',(20.5,12.5,6.4));
#11914=CARTESIAN_POINT('Origin',(20.,0.,5.1));
#11915=CARTESIAN_POINT('',(19.75,-3.06161699786838E-17,5.2));
#11916=CARTESIAN_POINT('Origin',(20.,0.,5.2));
#11917=CARTESIAN_POINT('',(19.75,3.06161699786838E-17,6.4));
#11918=CARTESIAN_POINT('',(19.75,-3.06161699786838E-17,5.1));
#11919=CARTESIAN_POINT('Origin',(20.,0.,6.4));
#11920=CARTESIAN_POINT('Origin',(25.5,8.1,5.1));
#11921=CARTESIAN_POINT('',(25.225,8.1,5.2));
#11922=CARTESIAN_POINT('Origin',(25.5,8.1,5.2));
#11923=CARTESIAN_POINT('',(25.225,8.1,6.4));
#11924=CARTESIAN_POINT('',(25.225,8.1,5.1));
#11925=CARTESIAN_POINT('Origin',(25.5,8.1,6.4));
#11926=CARTESIAN_POINT('Origin',(22.5,11.9,5.1));
#11927=CARTESIAN_POINT('',(22.225,11.9,5.2));
#11928=CARTESIAN_POINT('Origin',(22.5,11.9,5.2));
#11929=CARTESIAN_POINT('',(22.225,11.9,6.4));
#11930=CARTESIAN_POINT('',(22.225,11.9,5.1));
#11931=CARTESIAN_POINT('Origin',(22.5,11.9,6.4));
#11932=CARTESIAN_POINT('Origin',(22.5,8.1,5.1));
#11933=CARTESIAN_POINT('',(22.225,8.1,5.2));
#11934=CARTESIAN_POINT('Origin',(22.5,8.1,5.2));
#11935=CARTESIAN_POINT('',(22.225,8.1,6.4));
#11936=CARTESIAN_POINT('',(22.225,8.1,5.1));
#11937=CARTESIAN_POINT('Origin',(22.5,8.1,6.4));
#11938=CARTESIAN_POINT('Origin',(25.5,11.9,5.1));
#11939=CARTESIAN_POINT('',(25.225,11.9,5.2));
#11940=CARTESIAN_POINT('Origin',(25.5,11.9,5.2));
#11941=CARTESIAN_POINT('',(25.225,11.9,6.4));
#11942=CARTESIAN_POINT('',(25.225,11.9,5.1));
#11943=CARTESIAN_POINT('Origin',(25.5,11.9,6.4));
#11944=CARTESIAN_POINT('Origin',(17.5,8.1,5.1));
#11945=CARTESIAN_POINT('',(17.225,8.1,5.2));
#11946=CARTESIAN_POINT('Origin',(17.5,8.1,5.2));
#11947=CARTESIAN_POINT('',(17.225,8.1,6.4));
#11948=CARTESIAN_POINT('',(17.225,8.1,5.1));
#11949=CARTESIAN_POINT('Origin',(17.5,8.1,6.4));
#11950=CARTESIAN_POINT('Origin',(14.5,11.9,5.1));
#11951=CARTESIAN_POINT('',(14.225,11.9,5.2));
#11952=CARTESIAN_POINT('Origin',(14.5,11.9,5.2));
#11953=CARTESIAN_POINT('',(14.225,11.9,6.4));
#11954=CARTESIAN_POINT('',(14.225,11.9,5.1));
#11955=CARTESIAN_POINT('Origin',(14.5,11.9,6.4));
#11956=CARTESIAN_POINT('Origin',(14.5,8.1,5.1));
#11957=CARTESIAN_POINT('',(14.225,8.1,5.2));
#11958=CARTESIAN_POINT('Origin',(14.5,8.1,5.2));
#11959=CARTESIAN_POINT('',(14.225,8.1,6.4));
#11960=CARTESIAN_POINT('',(14.225,8.1,5.1));
#11961=CARTESIAN_POINT('Origin',(14.5,8.1,6.4));
#11962=CARTESIAN_POINT('Origin',(17.5,11.9,5.1));
#11963=CARTESIAN_POINT('',(17.225,11.9,5.2));
#11964=CARTESIAN_POINT('Origin',(17.5,11.9,5.2));
#11965=CARTESIAN_POINT('',(17.225,11.9,6.4));
#11966=CARTESIAN_POINT('',(17.225,11.9,5.1));
#11967=CARTESIAN_POINT('Origin',(17.5,11.9,6.4));
#11968=CARTESIAN_POINT('Origin',(25.5,-11.9,5.1));
#11969=CARTESIAN_POINT('',(25.225,-11.9,5.2));
#11970=CARTESIAN_POINT('Origin',(25.5,-11.9,5.2));
#11971=CARTESIAN_POINT('',(25.225,-11.9,6.4));
#11972=CARTESIAN_POINT('',(25.225,-11.9,5.1));
#11973=CARTESIAN_POINT('Origin',(25.5,-11.9,6.4));
#11974=CARTESIAN_POINT('Origin',(22.5,-8.1,5.1));
#11975=CARTESIAN_POINT('',(22.225,-8.1,5.2));
#11976=CARTESIAN_POINT('Origin',(22.5,-8.1,5.2));
#11977=CARTESIAN_POINT('',(22.225,-8.1,6.4));
#11978=CARTESIAN_POINT('',(22.225,-8.1,5.1));
#11979=CARTESIAN_POINT('Origin',(22.5,-8.1,6.4));
#11980=CARTESIAN_POINT('Origin',(22.5,-11.9,5.1));
#11981=CARTESIAN_POINT('',(22.225,-11.9,5.2));
#11982=CARTESIAN_POINT('Origin',(22.5,-11.9,5.2));
#11983=CARTESIAN_POINT('',(22.225,-11.9,6.4));
#11984=CARTESIAN_POINT('',(22.225,-11.9,5.1));
#11985=CARTESIAN_POINT('Origin',(22.5,-11.9,6.4));
#11986=CARTESIAN_POINT('Origin',(25.5,-8.1,5.1));
#11987=CARTESIAN_POINT('',(25.225,-8.1,5.2));
#11988=CARTESIAN_POINT('Origin',(25.5,-8.1,5.2));
#11989=CARTESIAN_POINT('',(25.225,-8.1,6.4));
#11990=CARTESIAN_POINT('',(25.225,-8.1,5.1));
#11991=CARTESIAN_POINT('Origin',(25.5,-8.1,6.4));
#11992=CARTESIAN_POINT('Origin',(17.5,-11.9,5.1));
#11993=CARTESIAN_POINT('',(17.225,-11.9,5.2));
#11994=CARTESIAN_POINT('Origin',(17.5,-11.9,5.2));
#11995=CARTESIAN_POINT('',(17.225,-11.9,6.4));
#11996=CARTESIAN_POINT('',(17.225,-11.9,5.1));
#11997=CARTESIAN_POINT('Origin',(17.5,-11.9,6.4));
#11998=CARTESIAN_POINT('Origin',(14.5,-8.1,5.1));
#11999=CARTESIAN_POINT('',(14.225,-8.1,5.2));
#12000=CARTESIAN_POINT('Origin',(14.5,-8.1,5.2));
#12001=CARTESIAN_POINT('',(14.225,-8.1,6.4));
#12002=CARTESIAN_POINT('',(14.225,-8.1,5.1));
#12003=CARTESIAN_POINT('Origin',(14.5,-8.1,6.4));
#12004=CARTESIAN_POINT('Origin',(14.5,-11.9,5.1));
#12005=CARTESIAN_POINT('',(14.225,-11.9,5.2));
#12006=CARTESIAN_POINT('Origin',(14.5,-11.9,5.2));
#12007=CARTESIAN_POINT('',(14.225,-11.9,6.4));
#12008=CARTESIAN_POINT('',(14.225,-11.9,5.1));
#12009=CARTESIAN_POINT('Origin',(14.5,-11.9,6.4));
#12010=CARTESIAN_POINT('Origin',(17.5,-8.1,5.1));
#12011=CARTESIAN_POINT('',(17.225,-8.1,5.2));
#12012=CARTESIAN_POINT('Origin',(17.5,-8.1,5.2));
#12013=CARTESIAN_POINT('',(17.225,-8.1,6.4));
#12014=CARTESIAN_POINT('',(17.225,-8.1,5.1));
#12015=CARTESIAN_POINT('Origin',(17.5,-8.1,6.4));
#12016=CARTESIAN_POINT('Origin',(28.,13.,5.2));
#12017=CARTESIAN_POINT('',(28.,13.,5.2));
#12018=CARTESIAN_POINT('',(12.,13.,5.2));
#12019=CARTESIAN_POINT('',(28.,13.,5.2));
#12020=CARTESIAN_POINT('',(12.,13.,6.4));
#12021=CARTESIAN_POINT('',(12.,13.,5.2));
#12022=CARTESIAN_POINT('',(28.,13.,6.4));
#12023=CARTESIAN_POINT('',(28.,13.,6.4));
#12024=CARTESIAN_POINT('',(28.,13.,5.2));
#12025=CARTESIAN_POINT('Origin',(28.,-13.,5.2));
#12026=CARTESIAN_POINT('',(28.,-13.,5.2));
#12027=CARTESIAN_POINT('',(28.,-13.,5.2));
#12028=CARTESIAN_POINT('',(28.,-13.,6.4));
#12029=CARTESIAN_POINT('',(28.,-13.,6.4));
#12030=CARTESIAN_POINT('',(28.,-13.,5.2));
#12031=CARTESIAN_POINT('Origin',(12.,-13.,5.2));
#12032=CARTESIAN_POINT('',(12.,-13.,5.2));
#12033=CARTESIAN_POINT('',(12.,-13.,5.2));
#12034=CARTESIAN_POINT('',(12.,-13.,6.4));
#12035=CARTESIAN_POINT('',(12.,-13.,6.4));
#12036=CARTESIAN_POINT('',(12.,-13.,5.2));
#12037=CARTESIAN_POINT('Origin',(12.,13.,5.2));
#12038=CARTESIAN_POINT('',(12.,13.,5.2));
#12039=CARTESIAN_POINT('',(12.,13.,6.4));
#12040=CARTESIAN_POINT('Origin',(20.,0.,6.4));
#12041=CARTESIAN_POINT('Origin',(20.,0.,5.2));
#12042=CARTESIAN_POINT('',(0.,0.,0.));
#12043=CARTESIAN_POINT('Origin',(20.,0.,6.4));
#12044=CARTESIAN_POINT('',(19.67,-4.04133443718624E-17,8.4));
#12045=CARTESIAN_POINT('Origin',(20.,0.,8.4));
#12046=CARTESIAN_POINT('',(19.67,-4.04133443718624E-17,6.4));
#12047=CARTESIAN_POINT('',(19.67,-4.04133443718624E-17,6.4));
#12048=CARTESIAN_POINT('Origin',(20.,0.,6.4));
#12049=CARTESIAN_POINT('Origin',(20.,0.,6.4));
#12050=CARTESIAN_POINT('',(18.5,-1.83697019872103E-16,8.4));
#12051=CARTESIAN_POINT('Origin',(20.,0.,8.4));
#12052=CARTESIAN_POINT('',(18.5,-1.83697019872103E-16,6.4));
#12053=CARTESIAN_POINT('',(18.5,-1.83697019872103E-16,6.4));
#12054=CARTESIAN_POINT('Origin',(20.,0.,6.4));
#12055=CARTESIAN_POINT('Origin',(20.,0.,8.4));
#12056=CARTESIAN_POINT('Origin',(20.,0.,6.4));
#12057=CARTESIAN_POINT('',(0.,0.,0.));
#12058=CARTESIAN_POINT('Origin',(19.5,12.5,6.3));
#12059=CARTESIAN_POINT('',(19.275,12.5,6.4));
#12060=CARTESIAN_POINT('Origin',(19.5,12.5,6.4));
#12061=CARTESIAN_POINT('',(19.275,12.5,6.6));
#12062=CARTESIAN_POINT('',(19.275,12.5,6.3));
#12063=CARTESIAN_POINT('Origin',(19.5,12.5,6.6));
#12064=CARTESIAN_POINT('Origin',(20.5,12.5,6.3));
#12065=CARTESIAN_POINT('',(20.275,12.5,6.4));
#12066=CARTESIAN_POINT('Origin',(20.5,12.5,6.4));
#12067=CARTESIAN_POINT('',(20.275,12.5,6.6));
#12068=CARTESIAN_POINT('',(20.275,12.5,6.3));
#12069=CARTESIAN_POINT('Origin',(20.5,12.5,6.6));
#12070=CARTESIAN_POINT('Origin',(19.,13.,6.6));
#12071=CARTESIAN_POINT('',(19.,13.,6.6));
#12072=CARTESIAN_POINT('',(19.,12.,6.6));
#12073=CARTESIAN_POINT('',(19.,13.,6.6));
#12074=CARTESIAN_POINT('',(21.,12.,6.6));
#12075=CARTESIAN_POINT('',(19.,12.,6.6));
#12076=CARTESIAN_POINT('',(21.,13.,6.6));
#12077=CARTESIAN_POINT('',(21.,13.,6.6));
#12078=CARTESIAN_POINT('',(19.,13.,6.6));
#12079=CARTESIAN_POINT('Origin',(19.,13.,8.));
#12080=CARTESIAN_POINT('',(19.,13.,8.));
#12081=CARTESIAN_POINT('',(19.,13.,8.));
#12082=CARTESIAN_POINT('',(21.,13.,8.));
#12083=CARTESIAN_POINT('',(21.,13.,8.));
#12084=CARTESIAN_POINT('',(19.,13.,8.));
#12085=CARTESIAN_POINT('Origin',(19.,13.2,8.));
#12086=CARTESIAN_POINT('',(19.,13.2,8.));
#12087=CARTESIAN_POINT('',(19.,13.2,8.));
#12088=CARTESIAN_POINT('',(21.,13.2,8.));
#12089=CARTESIAN_POINT('',(21.,13.2,8.));
#12090=CARTESIAN_POINT('',(19.,13.2,8.));
#12091=CARTESIAN_POINT('Origin',(19.,13.2,6.4));
#12092=CARTESIAN_POINT('',(19.,13.2,6.4));
#12093=CARTESIAN_POINT('',(19.,13.2,6.4));
#12094=CARTESIAN_POINT('',(21.,13.2,6.4));
#12095=CARTESIAN_POINT('',(21.,13.2,6.4));
#12096=CARTESIAN_POINT('',(19.,13.2,6.4));
#12097=CARTESIAN_POINT('Origin',(19.,12.,6.4));
#12098=CARTESIAN_POINT('',(19.,12.,6.4));
#12099=CARTESIAN_POINT('',(19.,12.,6.4));
#12100=CARTESIAN_POINT('',(21.,12.,6.4));
#12101=CARTESIAN_POINT('',(21.,12.,6.4));
#12102=CARTESIAN_POINT('',(19.,12.,6.4));
#12103=CARTESIAN_POINT('Origin',(19.,12.,6.6));
#12104=CARTESIAN_POINT('',(19.,12.,6.6));
#12105=CARTESIAN_POINT('',(21.,12.,6.6));
#12106=CARTESIAN_POINT('Origin',(21.,12.6,7.2));
#12107=CARTESIAN_POINT('Origin',(19.,12.6,7.2));
#12108=CARTESIAN_POINT('',(0.,0.,0.));
#12109=CARTESIAN_POINT('',(0.,0.,0.));
#12110=CARTESIAN_POINT('Origin',(1.5,-1.9,1.7));
#12111=CARTESIAN_POINT('',(1.56403124237433,-1.7,1.7));
#12112=CARTESIAN_POINT('',(1.43596875762567,-1.7,1.7));
#12113=CARTESIAN_POINT('',(0.75,-1.7,1.7));
#12114=CARTESIAN_POINT('Origin',(1.5,-1.9,1.7));
#12115=CARTESIAN_POINT('Origin',(1.5,-1.9,1.7));
#12116=CARTESIAN_POINT('',(1.56403124237433,-1.7,1.75));
#12117=CARTESIAN_POINT('',(1.56403124237433,-1.7,1.7));
#12118=CARTESIAN_POINT('',(1.29,-1.9,1.75));
#12119=CARTESIAN_POINT('Origin',(1.5,-1.9,1.75));
#12120=CARTESIAN_POINT('',(1.29,-1.9,2.4));
#12121=CARTESIAN_POINT('',(1.29,-1.9,1.7));
#12122=CARTESIAN_POINT('Origin',(1.5,-1.9,2.4));
#12123=CARTESIAN_POINT('',(1.43596875762567,-1.7,1.75));
#12124=CARTESIAN_POINT('Origin',(1.5,-1.9,1.75));
#12125=CARTESIAN_POINT('',(1.43596875762567,-1.7,1.7));
#12126=CARTESIAN_POINT('Origin',(-1.5,1.9,1.7));
#12127=CARTESIAN_POINT('',(-1.56403124237433,1.7,1.7));
#12128=CARTESIAN_POINT('',(-1.43596875762567,1.7,1.7));
#12129=CARTESIAN_POINT('',(-0.75,1.7,1.7));
#12130=CARTESIAN_POINT('Origin',(-1.5,1.9,1.7));
#12131=CARTESIAN_POINT('Origin',(-1.5,1.9,1.7));
#12132=CARTESIAN_POINT('',(-1.56403124237433,1.7,1.75));
#12133=CARTESIAN_POINT('',(-1.56403124237433,1.7,1.7));
#12134=CARTESIAN_POINT('',(-1.71,1.9,1.75));
#12135=CARTESIAN_POINT('Origin',(-1.5,1.9,1.75));
#12136=CARTESIAN_POINT('',(-1.71,1.9,2.4));
#12137=CARTESIAN_POINT('',(-1.71,1.9,1.7));
#12138=CARTESIAN_POINT('Origin',(-1.5,1.9,2.4));
#12139=CARTESIAN_POINT('',(-1.43596875762567,1.7,1.75));
#12140=CARTESIAN_POINT('Origin',(-1.5,1.9,1.75));
#12141=CARTESIAN_POINT('',(-1.43596875762567,1.7,1.7));
#12142=CARTESIAN_POINT('Origin',(-1.5,-1.9,1.7));
#12143=CARTESIAN_POINT('',(-1.43596875762567,-1.7,1.7));
#12144=CARTESIAN_POINT('',(-1.56403124237433,-1.7,1.7));
#12145=CARTESIAN_POINT('',(-0.75,-1.7,1.7));
#12146=CARTESIAN_POINT('Origin',(-1.5,-1.9,1.7));
#12147=CARTESIAN_POINT('Origin',(-1.5,-1.9,1.7));
#12148=CARTESIAN_POINT('',(-1.43596875762567,-1.7,1.75));
#12149=CARTESIAN_POINT('',(-1.43596875762567,-1.7,1.7));
#12150=CARTESIAN_POINT('',(-1.71,-1.9,1.75));
#12151=CARTESIAN_POINT('Origin',(-1.5,-1.9,1.75));
#12152=CARTESIAN_POINT('',(-1.71,-1.9,2.4));
#12153=CARTESIAN_POINT('',(-1.71,-1.9,1.7));
#12154=CARTESIAN_POINT('Origin',(-1.5,-1.9,2.4));
#12155=CARTESIAN_POINT('',(-1.56403124237433,-1.7,1.75));
#12156=CARTESIAN_POINT('Origin',(-1.5,-1.9,1.75));
#12157=CARTESIAN_POINT('',(-1.56403124237433,-1.7,1.7));
#12158=CARTESIAN_POINT('Origin',(1.5,1.9,1.7));
#12159=CARTESIAN_POINT('',(1.43596875762567,1.7,1.7));
#12160=CARTESIAN_POINT('',(1.56403124237433,1.7,1.7));
#12161=CARTESIAN_POINT('',(0.75,1.7,1.7));
#12162=CARTESIAN_POINT('Origin',(1.5,1.9,1.7));
#12163=CARTESIAN_POINT('Origin',(1.5,1.9,1.7));
#12164=CARTESIAN_POINT('',(1.43596875762567,1.7,1.75));
#12165=CARTESIAN_POINT('',(1.43596875762567,1.7,1.7));
#12166=CARTESIAN_POINT('',(1.29,1.9,1.75));
#12167=CARTESIAN_POINT('Origin',(1.5,1.9,1.75));
#12168=CARTESIAN_POINT('',(1.29,1.9,2.4));
#12169=CARTESIAN_POINT('',(1.29,1.9,1.7));
#12170=CARTESIAN_POINT('Origin',(1.5,1.9,2.4));
#12171=CARTESIAN_POINT('',(1.56403124237433,1.7,1.75));
#12172=CARTESIAN_POINT('Origin',(1.5,1.9,1.75));
#12173=CARTESIAN_POINT('',(1.56403124237433,1.7,1.7));
#12174=CARTESIAN_POINT('Origin',(0.,-1.7,1.75));
#12175=CARTESIAN_POINT('',(0.,-1.7,1.75));
#12176=CARTESIAN_POINT('',(-1.97,-1.7,1.75));
#12177=CARTESIAN_POINT('',(0.,-1.7,1.75));
#12178=CARTESIAN_POINT('',(-1.97,-1.7,0.43));
#12179=CARTESIAN_POINT('',(-1.97,-1.7,1.75));
#12180=CARTESIAN_POINT('',(1.97,-1.7,0.43));
#12181=CARTESIAN_POINT('',(0.,-1.7,0.43));
#12182=CARTESIAN_POINT('',(1.97,-1.7,1.75));
#12183=CARTESIAN_POINT('',(1.97,-1.7,1.75));
#12184=CARTESIAN_POINT('',(0.,-1.7,1.75));
#12185=CARTESIAN_POINT('Origin',(0.,1.7,0.43));
#12186=CARTESIAN_POINT('',(0.,1.7,1.75));
#12187=CARTESIAN_POINT('',(1.97,1.7,1.75));
#12188=CARTESIAN_POINT('',(0.,1.7,1.75));
#12189=CARTESIAN_POINT('',(1.97,1.7,0.43));
#12190=CARTESIAN_POINT('',(1.97,1.7,0.43));
#12191=CARTESIAN_POINT('',(-1.97,1.7,0.43));
#12192=CARTESIAN_POINT('',(0.,1.7,0.43));
#12193=CARTESIAN_POINT('',(-1.97,1.7,1.75));
#12194=CARTESIAN_POINT('',(-1.97,1.7,0.43));
#12195=CARTESIAN_POINT('',(0.,1.7,1.75));
#12196=CARTESIAN_POINT('Origin',(-1.97,0.,1.415));
#12197=CARTESIAN_POINT('',(-1.97,-2.35,1.75));
#12198=CARTESIAN_POINT('',(-1.97,-2.35,1.75));
#12199=CARTESIAN_POINT('',(-1.97,-2.35,2.4));
#12200=CARTESIAN_POINT('',(-1.97,-2.35,2.4));
#12201=CARTESIAN_POINT('',(-1.97,2.35,2.4));
#12202=CARTESIAN_POINT('',(-1.97,2.35,2.4));
#12203=CARTESIAN_POINT('',(-1.97,2.35,1.75));
#12204=CARTESIAN_POINT('',(-1.97,2.35,1.75));
#12205=CARTESIAN_POINT('',(-1.97,1.7,1.75));
#12206=CARTESIAN_POINT('',(-1.97,0.78,0.43));
#12207=CARTESIAN_POINT('',(-1.97,0.78,0.43));
#12208=CARTESIAN_POINT('',(-1.97,0.78,1.55));
#12209=CARTESIAN_POINT('',(-1.97,0.78,1.55));
#12210=CARTESIAN_POINT('',(-1.97,-0.78,1.55));
#12211=CARTESIAN_POINT('',(-1.97,-0.78,1.55));
#12212=CARTESIAN_POINT('',(-1.97,-0.78,0.43));
#12213=CARTESIAN_POINT('',(-1.97,-0.78,0.43));
#12214=CARTESIAN_POINT('',(-1.97,-1.7,0.43));
#12215=CARTESIAN_POINT('Origin',(0.,-2.35,1.75));
#12216=CARTESIAN_POINT('',(1.97,-2.35,1.75));
#12217=CARTESIAN_POINT('',(1.97,-2.35,1.75));
#12218=CARTESIAN_POINT('',(0.,-2.35,1.75));
#12219=CARTESIAN_POINT('Origin',(0.,-2.35,2.4));
#12220=CARTESIAN_POINT('',(1.97,-2.35,2.4));
#12221=CARTESIAN_POINT('',(1.97,-2.35,2.4));
#12222=CARTESIAN_POINT('',(0.,-2.35,2.4));
#12223=CARTESIAN_POINT('Origin',(0.,2.35,2.4));
#12224=CARTESIAN_POINT('',(1.97,2.35,2.4));
#12225=CARTESIAN_POINT('',(1.97,2.35,2.4));
#12226=CARTESIAN_POINT('',(0.,2.35,2.4));
#12227=CARTESIAN_POINT('Origin',(0.,2.35,1.75));
#12228=CARTESIAN_POINT('',(1.97,2.35,1.75));
#12229=CARTESIAN_POINT('',(1.97,2.35,1.75));
#12230=CARTESIAN_POINT('',(0.,2.35,1.75));
#12231=CARTESIAN_POINT('Origin',(0.,1.7,1.75));
#12232=CARTESIAN_POINT('',(1.97,1.7,1.75));
#12233=CARTESIAN_POINT('Origin',(0.,0.78,0.43));
#12234=CARTESIAN_POINT('',(1.97,0.78,0.43));
#12235=CARTESIAN_POINT('',(1.97,0.78,0.43));
#12236=CARTESIAN_POINT('',(0.,0.78,0.43));
#12237=CARTESIAN_POINT('Origin',(0.,0.78,1.55));
#12238=CARTESIAN_POINT('',(1.97,0.78,1.55));
#12239=CARTESIAN_POINT('',(1.97,0.78,1.55));
#12240=CARTESIAN_POINT('',(0.,0.78,1.55));
#12241=CARTESIAN_POINT('Origin',(0.,-0.78,1.55));
#12242=CARTESIAN_POINT('',(1.97,-0.78,1.55));
#12243=CARTESIAN_POINT('',(1.97,-0.78,1.55));
#12244=CARTESIAN_POINT('',(0.,-0.78,1.55));
#12245=CARTESIAN_POINT('Origin',(0.,-0.78,0.43));
#12246=CARTESIAN_POINT('',(1.97,-0.78,0.43));
#12247=CARTESIAN_POINT('',(1.97,-0.78,0.43));
#12248=CARTESIAN_POINT('',(0.,-0.78,0.43));
#12249=CARTESIAN_POINT('Origin',(0.,-1.7,0.43));
#12250=CARTESIAN_POINT('',(1.97,-1.7,0.43));
#12251=CARTESIAN_POINT('Origin',(1.97,0.,1.415));
#12252=CARTESIAN_POINT('',(0.,0.,0.));
#12253=CARTESIAN_POINT('Origin',(1.97,1.7,2.3));
#12254=CARTESIAN_POINT('',(1.97,1.7,2.3));
#12255=CARTESIAN_POINT('',(1.97,-1.7,2.3));
#12256=CARTESIAN_POINT('',(1.97,1.7,2.3));
#12257=CARTESIAN_POINT('',(3.07,-1.7,2.3));
#12258=CARTESIAN_POINT('',(1.97,-1.7,2.3));
#12259=CARTESIAN_POINT('',(3.07,1.7,2.3));
#12260=CARTESIAN_POINT('',(3.07,1.7,2.3));
#12261=CARTESIAN_POINT('',(1.97,1.7,2.3));
#12262=CARTESIAN_POINT('Origin',(1.97,1.7,0.46));
#12263=CARTESIAN_POINT('',(1.97,1.7,0.46));
#12264=CARTESIAN_POINT('',(1.97,1.7,0.46));
#12265=CARTESIAN_POINT('',(3.07,1.7,0.46));
#12266=CARTESIAN_POINT('',(3.07,1.7,0.46));
#12267=CARTESIAN_POINT('',(1.97,1.7,0.46));
#12268=CARTESIAN_POINT('Origin',(1.97,0.78,0.46));
#12269=CARTESIAN_POINT('',(1.97,0.78,0.46));
#12270=CARTESIAN_POINT('',(1.97,0.78,0.46));
#12271=CARTESIAN_POINT('',(3.07,0.78,0.46));
#12272=CARTESIAN_POINT('',(3.07,0.78,0.46));
#12273=CARTESIAN_POINT('',(1.97,0.78,0.46));
#12274=CARTESIAN_POINT('Origin',(1.97,0.78,1.55));
#12275=CARTESIAN_POINT('',(1.97,0.78,1.55));
#12276=CARTESIAN_POINT('',(1.97,0.78,1.55));
#12277=CARTESIAN_POINT('',(3.07,0.78,1.55));
#12278=CARTESIAN_POINT('',(3.07,0.78,1.55));
#12279=CARTESIAN_POINT('',(1.97,0.78,1.55));
#12280=CARTESIAN_POINT('Origin',(1.97,-0.78,1.55));
#12281=CARTESIAN_POINT('',(1.97,-0.78,1.55));
#12282=CARTESIAN_POINT('',(1.97,-0.78,1.55));
#12283=CARTESIAN_POINT('',(3.07,-0.78,1.55));
#12284=CARTESIAN_POINT('',(3.07,-0.78,1.55));
#12285=CARTESIAN_POINT('',(1.97,-0.78,1.55));
#12286=CARTESIAN_POINT('Origin',(1.97,-0.78,0.46));
#12287=CARTESIAN_POINT('',(1.97,-0.78,0.46));
#12288=CARTESIAN_POINT('',(1.97,-0.78,0.46));
#12289=CARTESIAN_POINT('',(3.07,-0.78,0.46));
#12290=CARTESIAN_POINT('',(3.07,-0.78,0.46));
#12291=CARTESIAN_POINT('',(1.97,-0.78,0.46));
#12292=CARTESIAN_POINT('Origin',(1.97,-1.7,0.46));
#12293=CARTESIAN_POINT('',(1.97,-1.7,0.46));
#12294=CARTESIAN_POINT('',(1.97,-1.7,0.46));
#12295=CARTESIAN_POINT('',(3.07,-1.7,0.46));
#12296=CARTESIAN_POINT('',(3.07,-1.7,0.46));
#12297=CARTESIAN_POINT('',(1.97,-1.7,0.46));
#12298=CARTESIAN_POINT('Origin',(1.97,-1.7,2.3));
#12299=CARTESIAN_POINT('',(1.97,-1.7,2.3));
#12300=CARTESIAN_POINT('',(3.07,-1.7,2.3));
#12301=CARTESIAN_POINT('Origin',(3.07,0.,1.38));
#12302=CARTESIAN_POINT('Origin',(1.97,0.,1.38));
#12303=CARTESIAN_POINT('',(0.,0.,0.));
#12304=CARTESIAN_POINT('Origin',(-1.97,-0.78,0.46));
#12305=CARTESIAN_POINT('',(-1.97,-1.7,0.46));
#12306=CARTESIAN_POINT('',(-1.97,-0.78,0.46));
#12307=CARTESIAN_POINT('',(-1.97,-1.7,0.46));
#12308=CARTESIAN_POINT('',(-3.07,-1.7,0.46));
#12309=CARTESIAN_POINT('',(-1.97,-1.7,0.46));
#12310=CARTESIAN_POINT('',(-3.07,-0.78,0.46));
#12311=CARTESIAN_POINT('',(-3.07,-1.7,0.46));
#12312=CARTESIAN_POINT('',(-1.97,-0.78,0.46));
#12313=CARTESIAN_POINT('Origin',(-1.97,-0.78,1.55));
#12314=CARTESIAN_POINT('',(-1.97,-0.78,1.55));
#12315=CARTESIAN_POINT('',(-1.97,-0.78,0.46));
#12316=CARTESIAN_POINT('',(-3.07,-0.78,1.55));
#12317=CARTESIAN_POINT('',(-3.07,-0.78,0.46));
#12318=CARTESIAN_POINT('',(-1.97,-0.78,1.55));
#12319=CARTESIAN_POINT('Origin',(-1.97,0.78,1.55));
#12320=CARTESIAN_POINT('',(-1.97,0.78,1.55));
#12321=CARTESIAN_POINT('',(-1.97,-0.78,1.55));
#12322=CARTESIAN_POINT('',(-3.07,0.78,1.55));
#12323=CARTESIAN_POINT('',(-3.07,-0.78,1.55));
#12324=CARTESIAN_POINT('',(-1.97,0.78,1.55));
#12325=CARTESIAN_POINT('Origin',(-1.97,0.78,0.46));
#12326=CARTESIAN_POINT('',(-1.97,0.78,0.46));
#12327=CARTESIAN_POINT('',(-1.97,0.78,1.55));
#12328=CARTESIAN_POINT('',(-3.07,0.78,0.46));
#12329=CARTESIAN_POINT('',(-3.07,0.78,1.55));
#12330=CARTESIAN_POINT('',(-1.97,0.78,0.46));
#12331=CARTESIAN_POINT('Origin',(-1.97,1.7,0.46));
#12332=CARTESIAN_POINT('',(-1.97,1.7,0.46));
#12333=CARTESIAN_POINT('',(-1.97,0.78,0.46));
#12334=CARTESIAN_POINT('',(-3.07,1.7,0.46));
#12335=CARTESIAN_POINT('',(-3.07,0.78,0.46));
#12336=CARTESIAN_POINT('',(-1.97,1.7,0.46));
#12337=CARTESIAN_POINT('Origin',(-1.97,1.7,2.3));
#12338=CARTESIAN_POINT('',(-1.97,1.7,2.3));
#12339=CARTESIAN_POINT('',(-1.97,1.7,0.46));
#12340=CARTESIAN_POINT('',(-3.07,1.7,2.3));
#12341=CARTESIAN_POINT('',(-3.07,1.7,0.46));
#12342=CARTESIAN_POINT('',(-1.97,1.7,2.3));
#12343=CARTESIAN_POINT('Origin',(-1.97,-1.7,2.3));
#12344=CARTESIAN_POINT('',(-1.97,-1.7,2.3));
#12345=CARTESIAN_POINT('',(-1.97,1.7,2.3));
#12346=CARTESIAN_POINT('',(-3.07,-1.7,2.3));
#12347=CARTESIAN_POINT('',(-3.07,1.7,2.3));
#12348=CARTESIAN_POINT('',(-1.97,-1.7,2.3));
#12349=CARTESIAN_POINT('Origin',(-1.97,-1.7,0.46));
#12350=CARTESIAN_POINT('',(-1.97,-1.7,2.3));
#12351=CARTESIAN_POINT('',(-3.07,-1.7,2.3));
#12352=CARTESIAN_POINT('Origin',(-1.97,0.,1.38));
#12353=CARTESIAN_POINT('Origin',(-3.07,0.,1.38));
#12354=CARTESIAN_POINT('',(0.,0.,0.));
#12355=CARTESIAN_POINT('',(0.,0.,0.));
#12356=CARTESIAN_POINT('',(0.,0.,0.));
#12357=CARTESIAN_POINT('',(0.,0.,0.));
#12358=CARTESIAN_POINT('Origin',(0.,0.09,0.));
#12359=CARTESIAN_POINT('',(-0.285,0.1,3.49024337756996E-17));
#12360=CARTESIAN_POINT('Origin',(0.,0.1,0.));
#12361=CARTESIAN_POINT('',(-0.265,0.08,-3.24531401774049E-17));
#12362=CARTESIAN_POINT('',(-0.275,0.09,3.36777869765522E-17));
#12363=CARTESIAN_POINT('Origin',(0.,0.08,0.));
#12364=CARTESIAN_POINT('Origin',(0.,0.,0.));
#12365=CARTESIAN_POINT('',(-0.265,0.,3.24531401774049E-17));
#12366=CARTESIAN_POINT('',(-0.265,0.,3.24531401774049E-17));
#12367=CARTESIAN_POINT('Origin',(0.,0.,0.));
#12368=CARTESIAN_POINT('Origin',(0.,0.1,0.));
#12369=CARTESIAN_POINT('',(-0.5,0.1,6.12323399573677E-17));
#12370=CARTESIAN_POINT('Origin',(0.,0.1,0.));
#12371=CARTESIAN_POINT('Origin',(0.,0.,0.));
#12372=CARTESIAN_POINT('',(-0.5,0.,6.12323399573677E-17));
#12373=CARTESIAN_POINT('',(-0.5,0.,6.12323399573677E-17));
#12374=CARTESIAN_POINT('Origin',(0.,0.,0.));
#12375=CARTESIAN_POINT('Origin',(0.,0.,0.));
#12376=CARTESIAN_POINT('',(0.,0.,0.));
#12377=CARTESIAN_POINT('',(0.,0.,0.));
#12378=CARTESIAN_POINT('',(0.,0.,0.));
#12379=CARTESIAN_POINT('',(0.,0.,0.));
#12380=CARTESIAN_POINT('',(0.,0.,0.));
#12381=CARTESIAN_POINT('',(0.,0.,0.));
#12382=CARTESIAN_POINT('',(0.,0.,0.));
#12383=CARTESIAN_POINT('',(0.,0.,0.));
#12384=CARTESIAN_POINT('',(0.,0.,0.));
#12385=CARTESIAN_POINT('',(0.,0.,0.));
#12386=CARTESIAN_POINT('',(0.,0.,0.));
#12387=CARTESIAN_POINT('',(0.,0.,0.));
#12388=CARTESIAN_POINT('',(0.,0.,0.));
#12389=CARTESIAN_POINT('',(0.,0.,0.));
#12390=CARTESIAN_POINT('',(0.,-10.,1.));
#12391=CARTESIAN_POINT('',(8.5,-10.,1.42));
#12392=CARTESIAN_POINT('',(8.5,-10.,2.8));
#12393=CARTESIAN_POINT('',(8.5,-10.,2.9));
#12394=CARTESIAN_POINT('',(31.5,-10.,1.42));
#12395=CARTESIAN_POINT('',(31.5,-10.,2.8));
#12396=CARTESIAN_POINT('',(31.5,-10.,2.9));
#12397=CARTESIAN_POINT('',(9.,-10.,2.8));
#12398=CARTESIAN_POINT('',(11.,-10.,3.77));
#12399=CARTESIAN_POINT('',(17.,-10.,3.77));
#12400=CARTESIAN_POINT('',(23.,-10.,3.77));
#12401=CARTESIAN_POINT('',(29.,-10.,3.77));
#12402=CARTESIAN_POINT('',(0.,10.,1.));
#12403=CARTESIAN_POINT('',(8.5,10.,1.42));
#12404=CARTESIAN_POINT('',(8.5,10.,2.8));
#12405=CARTESIAN_POINT('',(8.5,10.,2.9));
#12406=CARTESIAN_POINT('',(31.5,10.,1.42));
#12407=CARTESIAN_POINT('',(31.5,10.,2.8));
#12408=CARTESIAN_POINT('',(31.5,10.,2.9));
#12409=CARTESIAN_POINT('',(9.,10.,2.8));
#12410=CARTESIAN_POINT('',(11.,10.,3.77));
#12411=CARTESIAN_POINT('',(17.,10.,3.77));
#12412=CARTESIAN_POINT('',(23.,10.,3.77));
#12413=CARTESIAN_POINT('',(29.,10.,3.77));
#12414=CARTESIAN_POINT('',(1.,-10.,1.42));
#12415=CARTESIAN_POINT('',(1.,-10.,2.8));
#12416=CARTESIAN_POINT('',(1.,-10.,2.9));
#12417=CARTESIAN_POINT('',(1.,-10.,0.58));
#12418=CARTESIAN_POINT('',(1.,-10.,-0.8));
#12419=CARTESIAN_POINT('',(1.,-10.,-0.9));
#12420=CARTESIAN_POINT('',(1.,10.,1.42));
#12421=CARTESIAN_POINT('',(1.,10.,2.8));
#12422=CARTESIAN_POINT('',(1.,10.,2.9));
#12423=CARTESIAN_POINT('',(1.,10.,0.58));
#12424=CARTESIAN_POINT('',(1.,10.,-0.8));
#12425=CARTESIAN_POINT('',(1.,10.,-0.9));
#12426=CARTESIAN_POINT('',(39.,-10.,1.42));
#12427=CARTESIAN_POINT('',(39.,-10.,2.8));
#12428=CARTESIAN_POINT('',(39.,-10.,2.9));
#12429=CARTESIAN_POINT('',(39.,-10.,0.58));
#12430=CARTESIAN_POINT('',(39.,-10.,-0.8));
#12431=CARTESIAN_POINT('',(39.,-10.,-0.9));
#12432=CARTESIAN_POINT('',(39.,10.,1.42));
#12433=CARTESIAN_POINT('',(39.,10.,2.8));
#12434=CARTESIAN_POINT('',(39.,10.,2.9));
#12435=CARTESIAN_POINT('',(39.,10.,0.58));
#12436=CARTESIAN_POINT('',(39.,10.,-0.8));
#12437=CARTESIAN_POINT('',(39.,10.,-0.9));
#12438=CARTESIAN_POINT('',(7.5,-10.,1.42));
#12439=CARTESIAN_POINT('',(7.5,-10.,2.9));
#12440=CARTESIAN_POINT('',(7.5,10.,1.42));
#12441=CARTESIAN_POINT('',(7.5,10.,2.9));
#12442=CARTESIAN_POINT('',(32.5,-10.,1.42));
#12443=CARTESIAN_POINT('',(32.5,-10.,2.9));
#12444=CARTESIAN_POINT('',(32.5,10.,1.42));
#12445=CARTESIAN_POINT('',(32.5,10.,2.9));
#12446=CARTESIAN_POINT('',(0.,0.,0.));
#12447=CARTESIAN_POINT('Origin',(0.375,0.5,0.));
#12448=CARTESIAN_POINT('',(-0.375,0.5,-4.59242549680257E-17));
#12449=CARTESIAN_POINT('Origin',(0.,0.5,0.));
#12450=CARTESIAN_POINT('Origin',(0.,0.475,0.));
#12451=CARTESIAN_POINT('',(-0.425,0.45,-5.20474889637625E-17));
#12452=CARTESIAN_POINT('Origin',(0.,0.45,0.));
#12453=CARTESIAN_POINT('',(-0.4,0.475,-4.89858719658941E-17));
#12454=CARTESIAN_POINT('Origin',(0.,0.24,0.));
#12455=CARTESIAN_POINT('',(-0.425,0.0299999999999998,-5.20474889637625E-17));
#12456=CARTESIAN_POINT('Origin',(0.,0.0299999999999998,0.));
#12457=CARTESIAN_POINT('',(-0.425,0.24,-5.20474889637625E-17));
#12458=CARTESIAN_POINT('Origin',(0.,0.0150000000000001,0.));
#12459=CARTESIAN_POINT('',(-0.395,4.85722573273506E-17,-4.83735485663204E-17));
#12460=CARTESIAN_POINT('Origin',(0.,0.,0.));
#12461=CARTESIAN_POINT('',(-0.41,0.0150000000000001,-5.02105187650415E-17));
#12462=CARTESIAN_POINT('Origin',(0.27,0.,0.));
#12463=CARTESIAN_POINT('',(-0.27,0.,-3.30654635769785E-17));
#12464=CARTESIAN_POINT('Origin',(0.,0.,0.));
#12465=CARTESIAN_POINT('Origin',(0.,-0.02,0.));
#12466=CARTESIAN_POINT('',(-0.24505,-0.0498999999999999,3.00099698131059E-17));
#12467=CARTESIAN_POINT('Origin',(0.,-0.0498999999999999,0.));
#12468=CARTESIAN_POINT('',(-0.26,-0.02,-3.18408167778312E-17));
#12469=CARTESIAN_POINT('Origin',(0.,-0.995,0.));
#12470=CARTESIAN_POINT('',(-0.24505,-1.95495,3.00099698131059E-17));
#12471=CARTESIAN_POINT('Origin',(0.,-1.95495,0.));
#12472=CARTESIAN_POINT('',(-0.24505,-0.995,-3.00099698131059E-17));
#12473=CARTESIAN_POINT('Origin',(0.,-1.975,0.));
#12474=CARTESIAN_POINT('',(-0.2,-2.,-2.44929359829471E-17));
#12475=CARTESIAN_POINT('Origin',(0.,-2.,0.));
#12476=CARTESIAN_POINT('',(-0.225,-1.975,-2.75545529808154E-17));
#12477=CARTESIAN_POINT('Origin',(0.,-2.,0.));
#12478=CARTESIAN_POINT('Origin',(0.115470053837925,-0.5,-0.2));
#12479=CARTESIAN_POINT('',(0.23094010767585,-0.5,0.));
#12480=CARTESIAN_POINT('',(0.115470053837925,-0.5,-0.2));
#12481=CARTESIAN_POINT('',(0.23094010767585,-0.5,0.));
#12482=CARTESIAN_POINT('',(0.115470053837925,-0.8,-0.2));
#12483=CARTESIAN_POINT('',(0.115470053837925,-0.5,-0.2));
#12484=CARTESIAN_POINT('',(0.23094010767585,-0.8,0.));
#12485=CARTESIAN_POINT('',(0.23094010767585,-0.8,0.));
#12486=CARTESIAN_POINT('',(0.23094010767585,-0.5,0.));
#12487=CARTESIAN_POINT('Origin',(-0.115470053837925,-0.5,-0.2));
#12488=CARTESIAN_POINT('',(-0.115470053837925,-0.5,-0.2));
#12489=CARTESIAN_POINT('',(0.115470053837925,-0.5,-0.2));
#12490=CARTESIAN_POINT('',(-0.115470053837925,-0.8,-0.2));
#12491=CARTESIAN_POINT('',(-0.115470053837925,-0.5,-0.2));
#12492=CARTESIAN_POINT('',(0.115470053837925,-0.8,-0.2));
#12493=CARTESIAN_POINT('Origin',(-0.23094010767585,-0.5,-2.77555756156289E-17));
#12494=CARTESIAN_POINT('',(-0.23094010767585,-0.5,-2.82820063659975E-17));
#12495=CARTESIAN_POINT('',(-0.115470053837925,-0.5,-0.2));
#12496=CARTESIAN_POINT('',(-0.23094010767585,-0.8,-2.77555756156289E-17));
#12497=CARTESIAN_POINT('',(-0.23094010767585,-0.5,-2.82820063659975E-17));
#12498=CARTESIAN_POINT('',(-0.115470053837925,-0.8,-0.2));
#12499=CARTESIAN_POINT('Origin',(-0.115470053837925,-0.5,0.2));
#12500=CARTESIAN_POINT('',(-0.115470053837925,-0.5,0.2));
#12501=CARTESIAN_POINT('',(-0.23094010767585,-0.5,-2.82820063659975E-17));
#12502=CARTESIAN_POINT('',(-0.115470053837925,-0.8,0.2));
#12503=CARTESIAN_POINT('',(-0.115470053837925,-0.5,0.2));
#12504=CARTESIAN_POINT('',(-0.23094010767585,-0.8,-2.82820063659975E-17));
#12505=CARTESIAN_POINT('Origin',(0.115470053837925,-0.5,0.2));
#12506=CARTESIAN_POINT('',(0.115470053837925,-0.5,0.2));
#12507=CARTESIAN_POINT('',(-0.115470053837925,-0.5,0.2));
#12508=CARTESIAN_POINT('',(0.115470053837925,-0.8,0.2));
#12509=CARTESIAN_POINT('',(0.115470053837925,-0.5,0.2));
#12510=CARTESIAN_POINT('',(-0.115470053837925,-0.8,0.2));
#12511=CARTESIAN_POINT('Origin',(0.23094010767585,-0.5,0.));
#12512=CARTESIAN_POINT('',(0.115470053837925,-0.5,0.2));
#12513=CARTESIAN_POINT('',(0.115470053837925,-0.8,0.2));
#12514=CARTESIAN_POINT('Origin',(0.,-0.5,0.));
#12515=CARTESIAN_POINT('Origin',(0.,-0.8,0.));
#12516=CARTESIAN_POINT('',(0.,0.,0.));
#12517=CARTESIAN_POINT('Origin',(0.,0.,0.));
#12518=CARTESIAN_POINT('',(-0.32,0.16,3.91886975727153E-17));
#12519=CARTESIAN_POINT('Origin',(0.,0.16,0.));
#12520=CARTESIAN_POINT('',(-0.32,0.,3.91886975727153E-17));
#12521=CARTESIAN_POINT('',(-0.32,0.,3.91886975727153E-17));
#12522=CARTESIAN_POINT('Origin',(0.,0.,0.));
#12523=CARTESIAN_POINT('Origin',(0.,0.,0.));
#12524=CARTESIAN_POINT('',(-0.6,0.16,7.34788079488412E-17));
#12525=CARTESIAN_POINT('Origin',(0.,0.16,0.));
#12526=CARTESIAN_POINT('',(-0.6,0.,7.34788079488412E-17));
#12527=CARTESIAN_POINT('',(-0.6,0.,7.34788079488412E-17));
#12528=CARTESIAN_POINT('Origin',(0.,0.,0.));
#12529=CARTESIAN_POINT('Origin',(0.,0.16,0.));
#12530=CARTESIAN_POINT('Origin',(0.,0.,0.));
#12531=CARTESIAN_POINT('',(0.,0.,0.));
#12532=CARTESIAN_POINT('Origin',(0.45,0.6,0.));
#12533=CARTESIAN_POINT('',(-0.45,0.6,-5.51091059616309E-17));
#12534=CARTESIAN_POINT('Origin',(0.,0.6,0.));
#12535=CARTESIAN_POINT('Origin',(0.,0.575,0.));
#12536=CARTESIAN_POINT('',(-0.5,0.55,-6.12323399573677E-17));
#12537=CARTESIAN_POINT('Origin',(0.,0.55,0.));
#12538=CARTESIAN_POINT('',(-0.475,0.575,-5.81707229594993E-17));
#12539=CARTESIAN_POINT('Origin',(0.,0.29,0.));
#12540=CARTESIAN_POINT('',(-0.5,0.0299999999999998,-6.12323399573677E-17));
#12541=CARTESIAN_POINT('Origin',(0.,0.0299999999999998,0.));
#12542=CARTESIAN_POINT('',(-0.5,0.29,-6.12323399573677E-17));
#12543=CARTESIAN_POINT('Origin',(0.,0.0150000000000001,0.));
#12544=CARTESIAN_POINT('',(-0.47,7.11236625150491E-17,-5.75583995599256E-17));
#12545=CARTESIAN_POINT('Origin',(0.,0.,0.));
#12546=CARTESIAN_POINT('',(-0.485,0.0150000000000001,-5.93953697586466E-17));
#12547=CARTESIAN_POINT('Origin',(0.32,0.,0.));
#12548=CARTESIAN_POINT('',(-0.32,-6.93889390390723E-18,-3.91886975727153E-17));
#12549=CARTESIAN_POINT('Origin',(0.,0.,0.));
#12550=CARTESIAN_POINT('Origin',(0.,-0.02,0.));
#12551=CARTESIAN_POINT('',(-0.2942,-0.0515999999999999,3.60291088309151E-17));
#12552=CARTESIAN_POINT('Origin',(0.,-0.0515999999999999,0.));
#12553=CARTESIAN_POINT('',(-0.31,-0.02,-3.7964050773568E-17));
#12554=CARTESIAN_POINT('Origin',(0.,-1.24,0.));
#12555=CARTESIAN_POINT('',(-0.2942,-2.4458,3.60291088309151E-17));
#12556=CARTESIAN_POINT('Origin',(0.,-2.4458,0.));
#12557=CARTESIAN_POINT('',(-0.2942,-1.24,-3.60291088309151E-17));
#12558=CARTESIAN_POINT('Origin',(0.,-2.47,0.));
#12559=CARTESIAN_POINT('',(-0.24,-2.5,-2.93915231795365E-17));
#12560=CARTESIAN_POINT('Origin',(0.,-2.5,0.));
#12561=CARTESIAN_POINT('',(-0.27,-2.47,-3.30654635769785E-17));
#12562=CARTESIAN_POINT('Origin',(0.,-2.5,0.));
#12563=CARTESIAN_POINT('Origin',(0.144337567297406,-0.6,-0.25));
#12564=CARTESIAN_POINT('',(0.288675134594813,-0.6,0.));
#12565=CARTESIAN_POINT('',(0.144337567297406,-0.6,-0.25));
#12566=CARTESIAN_POINT('',(0.288675134594813,-0.6,0.));
#12567=CARTESIAN_POINT('',(0.144337567297406,-0.96,-0.25));
#12568=CARTESIAN_POINT('',(0.144337567297406,-0.6,-0.25));
#12569=CARTESIAN_POINT('',(0.288675134594813,-0.96,0.));
#12570=CARTESIAN_POINT('',(0.288675134594813,-0.96,0.));
#12571=CARTESIAN_POINT('',(0.288675134594813,-0.6,0.));
#12572=CARTESIAN_POINT('Origin',(-0.144337567297406,-0.6,-0.25));
#12573=CARTESIAN_POINT('',(-0.144337567297406,-0.6,-0.25));
#12574=CARTESIAN_POINT('',(0.144337567297406,-0.6,-0.25));
#12575=CARTESIAN_POINT('',(-0.144337567297406,-0.96,-0.25));
#12576=CARTESIAN_POINT('',(-0.144337567297406,-0.6,-0.25));
#12577=CARTESIAN_POINT('',(0.144337567297406,-0.96,-0.25));
#12578=CARTESIAN_POINT('Origin',(-0.288675134594813,-0.6,-8.32667268468867E-17));
#12579=CARTESIAN_POINT('',(-0.288675134594813,-0.6,-3.53525079574969E-17));
#12580=CARTESIAN_POINT('',(-0.144337567297406,-0.6,-0.25));
#12581=CARTESIAN_POINT('',(-0.288675134594813,-0.96,-5.55111512312578E-17));
#12582=CARTESIAN_POINT('',(-0.288675134594813,-0.6,-3.53525079574969E-17));
#12583=CARTESIAN_POINT('',(-0.144337567297406,-0.96,-0.25));
#12584=CARTESIAN_POINT('Origin',(-0.144337567297407,-0.6,0.25));
#12585=CARTESIAN_POINT('',(-0.144337567297407,-0.6,0.25));
#12586=CARTESIAN_POINT('',(-0.288675134594813,-0.6,-3.53525079574969E-17));
#12587=CARTESIAN_POINT('',(-0.144337567297407,-0.96,0.25));
#12588=CARTESIAN_POINT('',(-0.144337567297407,-0.6,0.25));
#12589=CARTESIAN_POINT('',(-0.288675134594813,-0.96,-3.53525079574969E-17));
#12590=CARTESIAN_POINT('Origin',(0.144337567297406,-0.6,0.25));
#12591=CARTESIAN_POINT('',(0.144337567297406,-0.6,0.25));
#12592=CARTESIAN_POINT('',(-0.144337567297407,-0.6,0.25));
#12593=CARTESIAN_POINT('',(0.144337567297406,-0.96,0.25));
#12594=CARTESIAN_POINT('',(0.144337567297406,-0.6,0.25));
#12595=CARTESIAN_POINT('',(-0.144337567297407,-0.96,0.25));
#12596=CARTESIAN_POINT('Origin',(0.288675134594813,-0.6,0.));
#12597=CARTESIAN_POINT('',(0.144337567297406,-0.6,0.25));
#12598=CARTESIAN_POINT('',(0.144337567297406,-0.96,0.25));
#12599=CARTESIAN_POINT('Origin',(0.,-0.6,0.));
#12600=CARTESIAN_POINT('Origin',(0.,-0.96,0.));
#12601=CARTESIAN_POINT('',(0.,0.,0.));
#12602=CARTESIAN_POINT('Origin',(0.,0.07,0.));
#12603=CARTESIAN_POINT('',(-0.235,0.08,2.87791997799628E-17));
#12604=CARTESIAN_POINT('Origin',(0.,0.08,0.));
#12605=CARTESIAN_POINT('',(-0.215,0.06,-2.63299061816681E-17));
#12606=CARTESIAN_POINT('',(-0.225,0.07,2.75545529808154E-17));
#12607=CARTESIAN_POINT('Origin',(0.,0.06,0.));
#12608=CARTESIAN_POINT('Origin',(0.,0.,0.));
#12609=CARTESIAN_POINT('',(-0.215,0.,2.63299061816681E-17));
#12610=CARTESIAN_POINT('',(-0.215,0.,2.63299061816681E-17));
#12611=CARTESIAN_POINT('Origin',(0.,0.,0.));
#12612=CARTESIAN_POINT('Origin',(0.,0.08,0.));
#12613=CARTESIAN_POINT('',(-0.45,0.08,5.51091059616309E-17));
#12614=CARTESIAN_POINT('Origin',(0.,0.08,0.));
#12615=CARTESIAN_POINT('Origin',(0.,0.,0.));
#12616=CARTESIAN_POINT('',(-0.45,0.,5.51091059616309E-17));
#12617=CARTESIAN_POINT('',(-0.45,0.,5.51091059616309E-17));
#12618=CARTESIAN_POINT('Origin',(0.,0.,0.));
#12619=CARTESIAN_POINT('Origin',(0.,0.,0.));
#12620=CARTESIAN_POINT('',(0.,0.,0.));
#12621=CARTESIAN_POINT('Origin',(0.0866025403784439,-0.4,-0.15));
#12622=CARTESIAN_POINT('',(0.173205080756888,-0.4,0.));
#12623=CARTESIAN_POINT('',(0.0866025403784439,-0.4,-0.15));
#12624=CARTESIAN_POINT('',(0.173205080756888,-0.4,0.));
#12625=CARTESIAN_POINT('',(0.0866025403784439,-0.64,-0.15));
#12626=CARTESIAN_POINT('',(0.0866025403784439,-0.4,-0.15));
#12627=CARTESIAN_POINT('',(0.173205080756888,-0.64,0.));
#12628=CARTESIAN_POINT('',(0.173205080756888,-0.64,0.));
#12629=CARTESIAN_POINT('',(0.173205080756888,-0.4,0.));
#12630=CARTESIAN_POINT('Origin',(-0.0866025403784438,-0.4,-0.15));
#12631=CARTESIAN_POINT('',(-0.0866025403784438,-0.4,-0.15));
#12632=CARTESIAN_POINT('',(0.0866025403784439,-0.4,-0.15));
#12633=CARTESIAN_POINT('',(-0.0866025403784438,-0.64,-0.15));
#12634=CARTESIAN_POINT('',(-0.0866025403784438,-0.4,-0.15));
#12635=CARTESIAN_POINT('',(0.0866025403784439,-0.64,-0.15));
#12636=CARTESIAN_POINT('Origin',(-0.173205080756888,-0.4,-2.77555756156289E-17));
#12637=CARTESIAN_POINT('',(-0.173205080756888,-0.4,-2.12115047744981E-17));
#12638=CARTESIAN_POINT('',(-0.0866025403784438,-0.4,-0.15));
#12639=CARTESIAN_POINT('',(-0.173205080756888,-0.64,-2.77555756156289E-17));
#12640=CARTESIAN_POINT('',(-0.173205080756888,-0.4,-2.12115047744981E-17));
#12641=CARTESIAN_POINT('',(-0.0866025403784438,-0.64,-0.15));
#12642=CARTESIAN_POINT('Origin',(-0.0866025403784439,-0.4,0.15));
#12643=CARTESIAN_POINT('',(-0.0866025403784439,-0.4,0.15));
#12644=CARTESIAN_POINT('',(-0.173205080756888,-0.4,-2.12115047744981E-17));
#12645=CARTESIAN_POINT('',(-0.0866025403784439,-0.64,0.15));
#12646=CARTESIAN_POINT('',(-0.0866025403784439,-0.4,0.15));
#12647=CARTESIAN_POINT('',(-0.173205080756888,-0.64,-2.12115047744981E-17));
#12648=CARTESIAN_POINT('Origin',(0.0866025403784439,-0.4,0.15));
#12649=CARTESIAN_POINT('',(0.0866025403784439,-0.4,0.15));
#12650=CARTESIAN_POINT('',(-0.0866025403784439,-0.4,0.15));
#12651=CARTESIAN_POINT('',(0.0866025403784439,-0.64,0.15));
#12652=CARTESIAN_POINT('',(0.0866025403784439,-0.4,0.15));
#12653=CARTESIAN_POINT('',(-0.0866025403784439,-0.64,0.15));
#12654=CARTESIAN_POINT('Origin',(0.173205080756888,-0.4,0.));
#12655=CARTESIAN_POINT('',(0.0866025403784439,-0.4,0.15));
#12656=CARTESIAN_POINT('',(0.0866025403784439,-0.64,0.15));
#12657=CARTESIAN_POINT('Origin',(0.,-0.4,-2.77555756156289E-17));
#12658=CARTESIAN_POINT('Origin',(0.,-0.64,-2.77555756156289E-17));
#12659=CARTESIAN_POINT('Origin',(0.,-1.,0.));
#12660=CARTESIAN_POINT('',(-0.1954,-1.,2.39295984553393E-17));
#12661=CARTESIAN_POINT('Origin',(0.,-1.,0.));
#12662=CARTESIAN_POINT('Origin',(0.3,0.4,0.));
#12663=CARTESIAN_POINT('',(-0.3,0.4,-3.67394039744206E-17));
#12664=CARTESIAN_POINT('Origin',(0.,0.4,0.));
#12665=CARTESIAN_POINT('Origin',(0.,0.375,0.));
#12666=CARTESIAN_POINT('',(-0.35,0.35,-4.28626379701573E-17));
#12667=CARTESIAN_POINT('Origin',(0.,0.35,0.));
#12668=CARTESIAN_POINT('',(-0.325,0.375,-3.9801020972289E-17));
#12669=CARTESIAN_POINT('Origin',(0.,0.19,0.));
#12670=CARTESIAN_POINT('',(-0.35,0.03,-4.28626379701574E-17));
#12671=CARTESIAN_POINT('Origin',(0.,0.03,0.));
#12672=CARTESIAN_POINT('',(-0.35,0.19,-4.28626379701574E-17));
#12673=CARTESIAN_POINT('Origin',(0.,0.0149999999999999,0.));
#12674=CARTESIAN_POINT('',(-0.32,-3.29597460435593E-17,-3.91886975727153E-17));
#12675=CARTESIAN_POINT('Origin',(0.,0.,0.));
#12676=CARTESIAN_POINT('',(-0.335,0.0149999999999999,-4.10256677714363E-17));
#12677=CARTESIAN_POINT('Origin',(0.22,0.,0.));
#12678=CARTESIAN_POINT('',(-0.22,-6.93889390390723E-18,-2.69422295812418E-17));
#12679=CARTESIAN_POINT('Origin',(0.,0.,0.));
#12680=CARTESIAN_POINT('Origin',(0.,-0.02,0.));
#12681=CARTESIAN_POINT('',(-0.1954,-0.0492,2.39295984553393E-17));
#12682=CARTESIAN_POINT('Origin',(0.,-0.0492,0.));
#12683=CARTESIAN_POINT('',(-0.21,-0.02,-2.57175827820944E-17));
#12684=CARTESIAN_POINT('Origin',(0.,-0.8,0.));
#12685=CARTESIAN_POINT('',(-0.1954,-0.8,-2.39295984553393E-17));
#12686=CARTESIAN_POINT('',(0.,0.,0.));
#12687=CARTESIAN_POINT('',(0.,0.,0.));
#12688=CARTESIAN_POINT('',(0.,0.,0.));
#12689=CARTESIAN_POINT('',(16.,-10.,2.8));
#12690=CARTESIAN_POINT('',(24.,-10.,2.8));
#12691=CARTESIAN_POINT('',(16.,10.,2.8));
#12692=CARTESIAN_POINT('',(24.,10.,2.8));
#12693=CARTESIAN_POINT('',(14.5,-11.9,6.4));
#12694=CARTESIAN_POINT('',(14.5,-11.9,6.5));
#12695=CARTESIAN_POINT('',(14.5,-8.1,6.4));
#12696=CARTESIAN_POINT('',(14.5,-8.1,6.5));
#12697=CARTESIAN_POINT('',(17.5,-11.9,6.4));
#12698=CARTESIAN_POINT('',(17.5,-11.9,6.5));
#12699=CARTESIAN_POINT('',(17.5,-8.1,6.4));
#12700=CARTESIAN_POINT('',(17.5,-8.1,6.5));
#12701=CARTESIAN_POINT('',(22.5,-11.9,6.4));
#12702=CARTESIAN_POINT('',(22.5,-11.9,6.5));
#12703=CARTESIAN_POINT('',(22.5,-8.1,6.4));
#12704=CARTESIAN_POINT('',(22.5,-8.1,6.5));
#12705=CARTESIAN_POINT('',(25.5,-11.9,6.4));
#12706=CARTESIAN_POINT('',(25.5,-11.9,6.5));
#12707=CARTESIAN_POINT('',(25.5,-8.1,6.4));
#12708=CARTESIAN_POINT('',(25.5,-8.1,6.5));
#12709=CARTESIAN_POINT('',(14.5,8.1,6.4));
#12710=CARTESIAN_POINT('',(14.5,8.1,6.5));
#12711=CARTESIAN_POINT('',(14.5,11.9,6.4));
#12712=CARTESIAN_POINT('',(14.5,11.9,6.5));
#12713=CARTESIAN_POINT('',(17.5,8.1,6.4));
#12714=CARTESIAN_POINT('',(17.5,8.1,6.5));
#12715=CARTESIAN_POINT('',(17.5,11.9,6.4));
#12716=CARTESIAN_POINT('',(17.5,11.9,6.5));
#12717=CARTESIAN_POINT('',(22.5,8.1,6.4));
#12718=CARTESIAN_POINT('',(22.5,8.1,6.5));
#12719=CARTESIAN_POINT('',(22.5,11.9,6.4));
#12720=CARTESIAN_POINT('',(22.5,11.9,6.5));
#12721=CARTESIAN_POINT('',(25.5,8.1,6.4));
#12722=CARTESIAN_POINT('',(25.5,8.1,6.5));
#12723=CARTESIAN_POINT('',(25.5,11.9,6.4));
#12724=CARTESIAN_POINT('',(25.5,11.9,6.5));
#12725=CARTESIAN_POINT('',(20.,0.,8.4));
#12726=CARTESIAN_POINT('',(20.,0.,8.56));
#12727=CARTESIAN_POINT('',(19.5,12.5,6.6));
#12728=CARTESIAN_POINT('',(19.5,12.5,6.68));
#12729=CARTESIAN_POINT('',(20.5,12.5,6.6));
#12730=CARTESIAN_POINT('',(20.5,12.5,6.68));
#12731=CARTESIAN_POINT('',(0.,0.,0.));
#12732=CARTESIAN_POINT('',(0.,0.,0.));
#12733=UNCERTAINTY_MEASURE_WITH_UNIT(LENGTH_MEASURE(0.001),#12805,
'DISTANCE_ACCURACY_VALUE',
'Maximum model space distance between geometric entities at asserted c
onnectivities');
#12734=UNCERTAINTY_MEASURE_WITH_UNIT(LENGTH_MEASURE(0.001),#12805,
'DISTANCE_ACCURACY_VALUE',
'Maximum model space distance between geometric entities at asserted c
onnectivities');
#12735=UNCERTAINTY_MEASURE_WITH_UNIT(LENGTH_MEASURE(0.001),#12805,
'DISTANCE_ACCURACY_VALUE',
'Maximum model space distance between geometric entities at asserted c
onnectivities');
#12736=UNCERTAINTY_MEASURE_WITH_UNIT(LENGTH_MEASURE(0.001),#12805,
'DISTANCE_ACCURACY_VALUE',
'Maximum model space distance between geometric entities at asserted c
onnectivities');
#12737=UNCERTAINTY_MEASURE_WITH_UNIT(LENGTH_MEASURE(0.001),#12805,
'DISTANCE_ACCURACY_VALUE',
'Maximum model space distance between geometric entities at asserted c
onnectivities');
#12738=UNCERTAINTY_MEASURE_WITH_UNIT(LENGTH_MEASURE(0.001),#12805,
'DISTANCE_ACCURACY_VALUE',
'Maximum model space distance between geometric entities at asserted c
onnectivities');
#12739=UNCERTAINTY_MEASURE_WITH_UNIT(LENGTH_MEASURE(0.001),#12805,
'DISTANCE_ACCURACY_VALUE',
'Maximum model space distance between geometric entities at asserted c
onnectivities');
#12740=UNCERTAINTY_MEASURE_WITH_UNIT(LENGTH_MEASURE(0.001),#12805,
'DISTANCE_ACCURACY_VALUE',
'Maximum model space distance between geometric entities at asserted c
onnectivities');
#12741=UNCERTAINTY_MEASURE_WITH_UNIT(LENGTH_MEASURE(0.001),#12805,
'DISTANCE_ACCURACY_VALUE',
'Maximum model space distance between geometric entities at asserted c
onnectivities');
#12742=UNCERTAINTY_MEASURE_WITH_UNIT(LENGTH_MEASURE(0.001),#12805,
'DISTANCE_ACCURACY_VALUE',
'Maximum model space distance between geometric entities at asserted c
onnectivities');
#12743=UNCERTAINTY_MEASURE_WITH_UNIT(LENGTH_MEASURE(0.001),#12805,
'DISTANCE_ACCURACY_VALUE',
'Maximum model space distance between geometric entities at asserted c
onnectivities');
#12744=UNCERTAINTY_MEASURE_WITH_UNIT(LENGTH_MEASURE(0.001),#12805,
'DISTANCE_ACCURACY_VALUE',
'Maximum model space distance between geometric entities at asserted c
onnectivities');
#12745=UNCERTAINTY_MEASURE_WITH_UNIT(LENGTH_MEASURE(0.001),#12805,
'DISTANCE_ACCURACY_VALUE',
'Maximum model space distance between geometric entities at asserted c
onnectivities');
#12746=UNCERTAINTY_MEASURE_WITH_UNIT(LENGTH_MEASURE(0.001),#12805,
'DISTANCE_ACCURACY_VALUE',
'Maximum model space distance between geometric entities at asserted c
onnectivities');
#12747=UNCERTAINTY_MEASURE_WITH_UNIT(LENGTH_MEASURE(0.001),#12805,
'DISTANCE_ACCURACY_VALUE',
'Maximum model space distance between geometric entities at asserted c
onnectivities');
#12748=UNCERTAINTY_MEASURE_WITH_UNIT(LENGTH_MEASURE(0.001),#12805,
'DISTANCE_ACCURACY_VALUE',
'Maximum model space distance between geometric entities at asserted c
onnectivities');
#12749=UNCERTAINTY_MEASURE_WITH_UNIT(LENGTH_MEASURE(0.001),#12805,
'DISTANCE_ACCURACY_VALUE',
'Maximum model space distance between geometric entities at asserted c
onnectivities');
#12750=UNCERTAINTY_MEASURE_WITH_UNIT(LENGTH_MEASURE(0.001),#12805,
'DISTANCE_ACCURACY_VALUE',
'Maximum model space distance between geometric entities at asserted c
onnectivities');
#12751=UNCERTAINTY_MEASURE_WITH_UNIT(LENGTH_MEASURE(0.001),#12805,
'DISTANCE_ACCURACY_VALUE',
'Maximum model space distance between geometric entities at asserted c
onnectivities');
#12752=UNCERTAINTY_MEASURE_WITH_UNIT(LENGTH_MEASURE(0.001),#12805,
'DISTANCE_ACCURACY_VALUE',
'Maximum model space distance between geometric entities at asserted c
onnectivities');
#12753=UNCERTAINTY_MEASURE_WITH_UNIT(LENGTH_MEASURE(0.001),#12805,
'DISTANCE_ACCURACY_VALUE',
'Maximum model space distance between geometric entities at asserted c
onnectivities');
#12754=UNCERTAINTY_MEASURE_WITH_UNIT(LENGTH_MEASURE(0.001),#12805,
'DISTANCE_ACCURACY_VALUE',
'Maximum model space distance between geometric entities at asserted c
onnectivities');
#12755=UNCERTAINTY_MEASURE_WITH_UNIT(LENGTH_MEASURE(0.001),#12805,
'DISTANCE_ACCURACY_VALUE',
'Maximum model space distance between geometric entities at asserted c
onnectivities');
#12756=UNCERTAINTY_MEASURE_WITH_UNIT(LENGTH_MEASURE(0.001),#12805,
'DISTANCE_ACCURACY_VALUE',
'Maximum model space distance between geometric entities at asserted c
onnectivities');
#12757=UNCERTAINTY_MEASURE_WITH_UNIT(LENGTH_MEASURE(0.001),#12805,
'DISTANCE_ACCURACY_VALUE',
'Maximum model space distance between geometric entities at asserted c
onnectivities');
#12758=UNCERTAINTY_MEASURE_WITH_UNIT(LENGTH_MEASURE(0.001),#12805,
'DISTANCE_ACCURACY_VALUE',
'Maximum model space distance between geometric entities at asserted c
onnectivities');
#12759=UNCERTAINTY_MEASURE_WITH_UNIT(LENGTH_MEASURE(0.001),#12805,
'DISTANCE_ACCURACY_VALUE',
'Maximum model space distance between geometric entities at asserted c
onnectivities');
#12760=UNCERTAINTY_MEASURE_WITH_UNIT(LENGTH_MEASURE(0.001),#12805,
'DISTANCE_ACCURACY_VALUE',
'Maximum model space distance between geometric entities at asserted c
onnectivities');
#12761=UNCERTAINTY_MEASURE_WITH_UNIT(LENGTH_MEASURE(0.001),#12805,
'DISTANCE_ACCURACY_VALUE',
'Maximum model space distance between geometric entities at asserted c
onnectivities');
#12762=UNCERTAINTY_MEASURE_WITH_UNIT(LENGTH_MEASURE(0.001),#12805,
'DISTANCE_ACCURACY_VALUE',
'Maximum model space distance between geometric entities at asserted c
onnectivities');
#12763=UNCERTAINTY_MEASURE_WITH_UNIT(LENGTH_MEASURE(0.001),#12805,
'DISTANCE_ACCURACY_VALUE',
'Maximum model space distance between geometric entities at asserted c
onnectivities');
#12764=UNCERTAINTY_MEASURE_WITH_UNIT(LENGTH_MEASURE(0.001),#12805,
'DISTANCE_ACCURACY_VALUE',
'Maximum model space distance between geometric entities at asserted c
onnectivities');
#12765=UNCERTAINTY_MEASURE_WITH_UNIT(LENGTH_MEASURE(0.001),#12805,
'DISTANCE_ACCURACY_VALUE',
'Maximum model space distance between geometric entities at asserted c
onnectivities');
#12766=UNCERTAINTY_MEASURE_WITH_UNIT(LENGTH_MEASURE(0.001),#12805,
'DISTANCE_ACCURACY_VALUE',
'Maximum model space distance between geometric entities at asserted c
onnectivities');
#12767=UNCERTAINTY_MEASURE_WITH_UNIT(LENGTH_MEASURE(0.001),#12805,
'DISTANCE_ACCURACY_VALUE',
'Maximum model space distance between geometric entities at asserted c
onnectivities');
#12768=UNCERTAINTY_MEASURE_WITH_UNIT(LENGTH_MEASURE(0.001),#12805,
'DISTANCE_ACCURACY_VALUE',
'Maximum model space distance between geometric entities at asserted c
onnectivities');
#12769=(
GEOMETRIC_REPRESENTATION_CONTEXT(3)
GLOBAL_UNCERTAINTY_ASSIGNED_CONTEXT((#12733))
GLOBAL_UNIT_ASSIGNED_CONTEXT((#12805,#12807,#12808))
REPRESENTATION_CONTEXT('','3D')
);
#12770=(
GEOMETRIC_REPRESENTATION_CONTEXT(3)
GLOBAL_UNCERTAINTY_ASSIGNED_CONTEXT((#12734))
GLOBAL_UNIT_ASSIGNED_CONTEXT((#12805,#12807,#12808))
REPRESENTATION_CONTEXT('','3D')
);
#12771=(
GEOMETRIC_REPRESENTATION_CONTEXT(3)
GLOBAL_UNCERTAINTY_ASSIGNED_CONTEXT((#12735))
GLOBAL_UNIT_ASSIGNED_CONTEXT((#12805,#12807,#12808))
REPRESENTATION_CONTEXT('','3D')
);
#12772=(
GEOMETRIC_REPRESENTATION_CONTEXT(3)
GLOBAL_UNCERTAINTY_ASSIGNED_CONTEXT((#12736))
GLOBAL_UNIT_ASSIGNED_CONTEXT((#12805,#12807,#12808))
REPRESENTATION_CONTEXT('','3D')
);
#12773=(
GEOMETRIC_REPRESENTATION_CONTEXT(3)
GLOBAL_UNCERTAINTY_ASSIGNED_CONTEXT((#12737))
GLOBAL_UNIT_ASSIGNED_CONTEXT((#12805,#12807,#12808))
REPRESENTATION_CONTEXT('','3D')
);
#12774=(
GEOMETRIC_REPRESENTATION_CONTEXT(3)
GLOBAL_UNCERTAINTY_ASSIGNED_CONTEXT((#12738))
GLOBAL_UNIT_ASSIGNED_CONTEXT((#12805,#12807,#12808))
REPRESENTATION_CONTEXT('','3D')
);
#12775=(
GEOMETRIC_REPRESENTATION_CONTEXT(3)
GLOBAL_UNCERTAINTY_ASSIGNED_CONTEXT((#12739))
GLOBAL_UNIT_ASSIGNED_CONTEXT((#12805,#12807,#12808))
REPRESENTATION_CONTEXT('','3D')
);
#12776=(
GEOMETRIC_REPRESENTATION_CONTEXT(3)
GLOBAL_UNCERTAINTY_ASSIGNED_CONTEXT((#12740))
GLOBAL_UNIT_ASSIGNED_CONTEXT((#12805,#12807,#12808))
REPRESENTATION_CONTEXT('','3D')
);
#12777=(
GEOMETRIC_REPRESENTATION_CONTEXT(3)
GLOBAL_UNCERTAINTY_ASSIGNED_CONTEXT((#12741))
GLOBAL_UNIT_ASSIGNED_CONTEXT((#12805,#12807,#12808))
REPRESENTATION_CONTEXT('','3D')
);
#12778=(
GEOMETRIC_REPRESENTATION_CONTEXT(3)
GLOBAL_UNCERTAINTY_ASSIGNED_CONTEXT((#12742))
GLOBAL_UNIT_ASSIGNED_CONTEXT((#12805,#12807,#12808))
REPRESENTATION_CONTEXT('','3D')
);
#12779=(
GEOMETRIC_REPRESENTATION_CONTEXT(3)
GLOBAL_UNCERTAINTY_ASSIGNED_CONTEXT((#12743))
GLOBAL_UNIT_ASSIGNED_CONTEXT((#12805,#12807,#12808))
REPRESENTATION_CONTEXT('','3D')
);
#12780=(
GEOMETRIC_REPRESENTATION_CONTEXT(3)
GLOBAL_UNCERTAINTY_ASSIGNED_CONTEXT((#12744))
GLOBAL_UNIT_ASSIGNED_CONTEXT((#12805,#12807,#12808))
REPRESENTATION_CONTEXT('','3D')
);
#12781=(
GEOMETRIC_REPRESENTATION_CONTEXT(3)
GLOBAL_UNCERTAINTY_ASSIGNED_CONTEXT((#12745))
GLOBAL_UNIT_ASSIGNED_CONTEXT((#12805,#12807,#12808))
REPRESENTATION_CONTEXT('','3D')
);
#12782=(
GEOMETRIC_REPRESENTATION_CONTEXT(3)
GLOBAL_UNCERTAINTY_ASSIGNED_CONTEXT((#12746))
GLOBAL_UNIT_ASSIGNED_CONTEXT((#12805,#12807,#12808))
REPRESENTATION_CONTEXT('','3D')
);
#12783=(
GEOMETRIC_REPRESENTATION_CONTEXT(3)
GLOBAL_UNCERTAINTY_ASSIGNED_CONTEXT((#12747))
GLOBAL_UNIT_ASSIGNED_CONTEXT((#12805,#12807,#12808))
REPRESENTATION_CONTEXT('','3D')
);
#12784=(
GEOMETRIC_REPRESENTATION_CONTEXT(3)
GLOBAL_UNCERTAINTY_ASSIGNED_CONTEXT((#12748))
GLOBAL_UNIT_ASSIGNED_CONTEXT((#12805,#12807,#12808))
REPRESENTATION_CONTEXT('','3D')
);
#12785=(
GEOMETRIC_REPRESENTATION_CONTEXT(3)
GLOBAL_UNCERTAINTY_ASSIGNED_CONTEXT((#12749))
GLOBAL_UNIT_ASSIGNED_CONTEXT((#12805,#12807,#12808))
REPRESENTATION_CONTEXT('','3D')
);
#12786=(
GEOMETRIC_REPRESENTATION_CONTEXT(3)
GLOBAL_UNCERTAINTY_ASSIGNED_CONTEXT((#12750))
GLOBAL_UNIT_ASSIGNED_CONTEXT((#12805,#12807,#12808))
REPRESENTATION_CONTEXT('','3D')
);
#12787=(
GEOMETRIC_REPRESENTATION_CONTEXT(3)
GLOBAL_UNCERTAINTY_ASSIGNED_CONTEXT((#12751))
GLOBAL_UNIT_ASSIGNED_CONTEXT((#12805,#12807,#12808))
REPRESENTATION_CONTEXT('','3D')
);
#12788=(
GEOMETRIC_REPRESENTATION_CONTEXT(3)
GLOBAL_UNCERTAINTY_ASSIGNED_CONTEXT((#12752))
GLOBAL_UNIT_ASSIGNED_CONTEXT((#12805,#12807,#12808))
REPRESENTATION_CONTEXT('','3D')
);
#12789=(
GEOMETRIC_REPRESENTATION_CONTEXT(3)
GLOBAL_UNCERTAINTY_ASSIGNED_CONTEXT((#12753))
GLOBAL_UNIT_ASSIGNED_CONTEXT((#12805,#12807,#12808))
REPRESENTATION_CONTEXT('','3D')
);
#12790=(
GEOMETRIC_REPRESENTATION_CONTEXT(3)
GLOBAL_UNCERTAINTY_ASSIGNED_CONTEXT((#12754))
GLOBAL_UNIT_ASSIGNED_CONTEXT((#12805,#12807,#12808))
REPRESENTATION_CONTEXT('','3D')
);
#12791=(
GEOMETRIC_REPRESENTATION_CONTEXT(3)
GLOBAL_UNCERTAINTY_ASSIGNED_CONTEXT((#12755))
GLOBAL_UNIT_ASSIGNED_CONTEXT((#12805,#12807,#12808))
REPRESENTATION_CONTEXT('','3D')
);
#12792=(
GEOMETRIC_REPRESENTATION_CONTEXT(3)
GLOBAL_UNCERTAINTY_ASSIGNED_CONTEXT((#12756))
GLOBAL_UNIT_ASSIGNED_CONTEXT((#12805,#12807,#12808))
REPRESENTATION_CONTEXT('','3D')
);
#12793=(
GEOMETRIC_REPRESENTATION_CONTEXT(3)
GLOBAL_UNCERTAINTY_ASSIGNED_CONTEXT((#12757))
GLOBAL_UNIT_ASSIGNED_CONTEXT((#12805,#12807,#12808))
REPRESENTATION_CONTEXT('','3D')
);
#12794=(
GEOMETRIC_REPRESENTATION_CONTEXT(3)
GLOBAL_UNCERTAINTY_ASSIGNED_CONTEXT((#12758))
GLOBAL_UNIT_ASSIGNED_CONTEXT((#12805,#12807,#12808))
REPRESENTATION_CONTEXT('','3D')
);
#12795=(
GEOMETRIC_REPRESENTATION_CONTEXT(3)
GLOBAL_UNCERTAINTY_ASSIGNED_CONTEXT((#12759))
GLOBAL_UNIT_ASSIGNED_CONTEXT((#12805,#12807,#12808))
REPRESENTATION_CONTEXT('','3D')
);
#12796=(
GEOMETRIC_REPRESENTATION_CONTEXT(3)
GLOBAL_UNCERTAINTY_ASSIGNED_CONTEXT((#12760))
GLOBAL_UNIT_ASSIGNED_CONTEXT((#12805,#12807,#12808))
REPRESENTATION_CONTEXT('','3D')
);
#12797=(
GEOMETRIC_REPRESENTATION_CONTEXT(3)
GLOBAL_UNCERTAINTY_ASSIGNED_CONTEXT((#12761))
GLOBAL_UNIT_ASSIGNED_CONTEXT((#12805,#12807,#12808))
REPRESENTATION_CONTEXT('','3D')
);
#12798=(
GEOMETRIC_REPRESENTATION_CONTEXT(3)
GLOBAL_UNCERTAINTY_ASSIGNED_CONTEXT((#12762))
GLOBAL_UNIT_ASSIGNED_CONTEXT((#12805,#12807,#12808))
REPRESENTATION_CONTEXT('','3D')
);
#12799=(
GEOMETRIC_REPRESENTATION_CONTEXT(3)
GLOBAL_UNCERTAINTY_ASSIGNED_CONTEXT((#12763))
GLOBAL_UNIT_ASSIGNED_CONTEXT((#12805,#12807,#12808))
REPRESENTATION_CONTEXT('','3D')
);
#12800=(
GEOMETRIC_REPRESENTATION_CONTEXT(3)
GLOBAL_UNCERTAINTY_ASSIGNED_CONTEXT((#12764))
GLOBAL_UNIT_ASSIGNED_CONTEXT((#12805,#12807,#12808))
REPRESENTATION_CONTEXT('','3D')
);
#12801=(
GEOMETRIC_REPRESENTATION_CONTEXT(3)
GLOBAL_UNCERTAINTY_ASSIGNED_CONTEXT((#12765))
GLOBAL_UNIT_ASSIGNED_CONTEXT((#12805,#12807,#12808))
REPRESENTATION_CONTEXT('','3D')
);
#12802=(
GEOMETRIC_REPRESENTATION_CONTEXT(3)
GLOBAL_UNCERTAINTY_ASSIGNED_CONTEXT((#12766))
GLOBAL_UNIT_ASSIGNED_CONTEXT((#12805,#12807,#12808))
REPRESENTATION_CONTEXT('','3D')
);
#12803=(
GEOMETRIC_REPRESENTATION_CONTEXT(3)
GLOBAL_UNCERTAINTY_ASSIGNED_CONTEXT((#12767))
GLOBAL_UNIT_ASSIGNED_CONTEXT((#12805,#12807,#12808))
REPRESENTATION_CONTEXT('','3D')
);
#12804=(
GEOMETRIC_REPRESENTATION_CONTEXT(3)
GLOBAL_UNCERTAINTY_ASSIGNED_CONTEXT((#12768))
GLOBAL_UNIT_ASSIGNED_CONTEXT((#12805,#12807,#12808))
REPRESENTATION_CONTEXT('','3D')
);
#12805=(
LENGTH_UNIT()
NAMED_UNIT(*)
SI_UNIT(.CENTI.,.METRE.)
);
#12806=(
LENGTH_UNIT()
NAMED_UNIT(*)
SI_UNIT($,.METRE.)
);
#12807=(
NAMED_UNIT(*)
PLANE_ANGLE_UNIT()
SI_UNIT($,.RADIAN.)
);
#12808=(
NAMED_UNIT(*)
SI_UNIT($,.STERADIAN.)
SOLID_ANGLE_UNIT()
);
#12809=SHAPE_DEFINITION_REPRESENTATION(#12844,#12999);
#12810=SHAPE_DEFINITION_REPRESENTATION(#12845,#13000);
#12811=SHAPE_DEFINITION_REPRESENTATION(#12846,#13001);
#12812=SHAPE_DEFINITION_REPRESENTATION(#12847,#13002);
#12813=SHAPE_DEFINITION_REPRESENTATION(#12848,#13003);
#12814=SHAPE_DEFINITION_REPRESENTATION(#12849,#13004);
#12815=SHAPE_DEFINITION_REPRESENTATION(#12850,#13005);
#12816=SHAPE_DEFINITION_REPRESENTATION(#12851,#13006);
#12817=SHAPE_DEFINITION_REPRESENTATION(#12852,#13007);
#12818=SHAPE_DEFINITION_REPRESENTATION(#12853,#13008);
#12819=SHAPE_DEFINITION_REPRESENTATION(#12854,#13009);
#12820=SHAPE_DEFINITION_REPRESENTATION(#12855,#13010);
#12821=SHAPE_DEFINITION_REPRESENTATION(#12856,#13011);
#12822=SHAPE_DEFINITION_REPRESENTATION(#12857,#13012);
#12823=SHAPE_DEFINITION_REPRESENTATION(#12858,#13013);
#12824=SHAPE_DEFINITION_REPRESENTATION(#12859,#13014);
#12825=SHAPE_DEFINITION_REPRESENTATION(#12860,#13015);
#12826=SHAPE_DEFINITION_REPRESENTATION(#12861,#13016);
#12827=SHAPE_DEFINITION_REPRESENTATION(#12862,#13017);
#12828=SHAPE_DEFINITION_REPRESENTATION(#12863,#13018);
#12829=SHAPE_DEFINITION_REPRESENTATION(#12864,#13019);
#12830=SHAPE_DEFINITION_REPRESENTATION(#12865,#13020);
#12831=SHAPE_DEFINITION_REPRESENTATION(#12866,#13021);
#12832=SHAPE_DEFINITION_REPRESENTATION(#12867,#13022);
#12833=SHAPE_DEFINITION_REPRESENTATION(#12868,#13023);
#12834=SHAPE_DEFINITION_REPRESENTATION(#12869,#13024);
#12835=SHAPE_DEFINITION_REPRESENTATION(#12870,#13025);
#12836=SHAPE_DEFINITION_REPRESENTATION(#12871,#13026);
#12837=SHAPE_DEFINITION_REPRESENTATION(#12872,#13027);
#12838=SHAPE_DEFINITION_REPRESENTATION(#12876,#13028);
#12839=SHAPE_DEFINITION_REPRESENTATION(#12947,#13029);
#12840=SHAPE_DEFINITION_REPRESENTATION(#12948,#13030);
#12841=SHAPE_DEFINITION_REPRESENTATION(#12949,#13031);
#12842=SHAPE_DEFINITION_REPRESENTATION(#12950,#13032);
#12843=SHAPE_DEFINITION_REPRESENTATION(#12951,#13033);
#12844=PRODUCT_DEFINITION_SHAPE('',$,#13035);
#12845=PRODUCT_DEFINITION_SHAPE('',$,#13036);
#12846=PRODUCT_DEFINITION_SHAPE('',$,#13037);
#12847=PRODUCT_DEFINITION_SHAPE('',$,#13038);
#12848=PRODUCT_DEFINITION_SHAPE('',$,#13039);
#12849=PRODUCT_DEFINITION_SHAPE('',$,#13040);
#12850=PRODUCT_DEFINITION_SHAPE('',$,#13041);
#12851=PRODUCT_DEFINITION_SHAPE('',$,#13042);
#12852=PRODUCT_DEFINITION_SHAPE('',$,#13043);
#12853=PRODUCT_DEFINITION_SHAPE('',$,#13044);
#12854=PRODUCT_DEFINITION_SHAPE('',$,#13045);
#12855=PRODUCT_DEFINITION_SHAPE('',$,#13046);
#12856=PRODUCT_DEFINITION_SHAPE('',$,#13047);
#12857=PRODUCT_DEFINITION_SHAPE('',$,#13048);
#12858=PRODUCT_DEFINITION_SHAPE('',$,#13049);
#12859=PRODUCT_DEFINITION_SHAPE('',$,#13050);
#12860=PRODUCT_DEFINITION_SHAPE('',$,#13051);
#12861=PRODUCT_DEFINITION_SHAPE('',$,#13052);
#12862=PRODUCT_DEFINITION_SHAPE('',$,#13053);
#12863=PRODUCT_DEFINITION_SHAPE('',$,#13054);
#12864=PRODUCT_DEFINITION_SHAPE('',$,#13055);
#12865=PRODUCT_DEFINITION_SHAPE('',$,#13056);
#12866=PRODUCT_DEFINITION_SHAPE('',$,#13057);
#12867=PRODUCT_DEFINITION_SHAPE('',$,#13058);
#12868=PRODUCT_DEFINITION_SHAPE('',$,#13059);
#12869=PRODUCT_DEFINITION_SHAPE('',$,#13060);
#12870=PRODUCT_DEFINITION_SHAPE('',$,#13061);
#12871=PRODUCT_DEFINITION_SHAPE('',$,#13062);
#12872=PRODUCT_DEFINITION_SHAPE('',$,#13063);
#12873=PRODUCT_DEFINITION_SHAPE($,$,#371);
#12874=PRODUCT_DEFINITION_SHAPE($,$,#372);
#12875=PRODUCT_DEFINITION_SHAPE($,$,#373);
#12876=PRODUCT_DEFINITION_SHAPE('',$,#13064);
#12877=PRODUCT_DEFINITION_SHAPE($,$,#374);
#12878=PRODUCT_DEFINITION_SHAPE($,$,#375);
#12879=PRODUCT_DEFINITION_SHAPE($,$,#376);
#12880=PRODUCT_DEFINITION_SHAPE($,$,#377);
#12881=PRODUCT_DEFINITION_SHAPE($,$,#378);
#12882=PRODUCT_DEFINITION_SHAPE($,$,#379);
#12883=PRODUCT_DEFINITION_SHAPE($,$,#380);
#12884=PRODUCT_DEFINITION_SHAPE($,$,#381);
#12885=PRODUCT_DEFINITION_SHAPE($,$,#382);
#12886=PRODUCT_DEFINITION_SHAPE($,$,#383);
#12887=PRODUCT_DEFINITION_SHAPE($,$,#384);
#12888=PRODUCT_DEFINITION_SHAPE($,$,#385);
#12889=PRODUCT_DEFINITION_SHAPE($,$,#386);
#12890=PRODUCT_DEFINITION_SHAPE($,$,#387);
#12891=PRODUCT_DEFINITION_SHAPE($,$,#388);
#12892=PRODUCT_DEFINITION_SHAPE($,$,#389);
#12893=PRODUCT_DEFINITION_SHAPE($,$,#390);
#12894=PRODUCT_DEFINITION_SHAPE($,$,#391);
#12895=PRODUCT_DEFINITION_SHAPE($,$,#392);
#12896=PRODUCT_DEFINITION_SHAPE($,$,#393);
#12897=PRODUCT_DEFINITION_SHAPE($,$,#394);
#12898=PRODUCT_DEFINITION_SHAPE($,$,#395);
#12899=PRODUCT_DEFINITION_SHAPE($,$,#396);
#12900=PRODUCT_DEFINITION_SHAPE($,$,#397);
#12901=PRODUCT_DEFINITION_SHAPE($,$,#398);
#12902=PRODUCT_DEFINITION_SHAPE($,$,#399);
#12903=PRODUCT_DEFINITION_SHAPE($,$,#400);
#12904=PRODUCT_DEFINITION_SHAPE($,$,#401);
#12905=PRODUCT_DEFINITION_SHAPE($,$,#402);
#12906=PRODUCT_DEFINITION_SHAPE($,$,#403);
#12907=PRODUCT_DEFINITION_SHAPE($,$,#404);
#12908=PRODUCT_DEFINITION_SHAPE($,$,#405);
#12909=PRODUCT_DEFINITION_SHAPE($,$,#406);
#12910=PRODUCT_DEFINITION_SHAPE($,$,#407);
#12911=PRODUCT_DEFINITION_SHAPE($,$,#408);
#12912=PRODUCT_DEFINITION_SHAPE($,$,#409);
#12913=PRODUCT_DEFINITION_SHAPE($,$,#410);
#12914=PRODUCT_DEFINITION_SHAPE($,$,#411);
#12915=PRODUCT_DEFINITION_SHAPE($,$,#412);
#12916=PRODUCT_DEFINITION_SHAPE($,$,#413);
#12917=PRODUCT_DEFINITION_SHAPE($,$,#414);
#12918=PRODUCT_DEFINITION_SHAPE($,$,#415);
#12919=PRODUCT_DEFINITION_SHAPE($,$,#416);
#12920=PRODUCT_DEFINITION_SHAPE($,$,#417);
#12921=PRODUCT_DEFINITION_SHAPE($,$,#418);
#12922=PRODUCT_DEFINITION_SHAPE($,$,#419);
#12923=PRODUCT_DEFINITION_SHAPE($,$,#420);
#12924=PRODUCT_DEFINITION_SHAPE($,$,#421);
#12925=PRODUCT_DEFINITION_SHAPE($,$,#422);
#12926=PRODUCT_DEFINITION_SHAPE($,$,#423);
#12927=PRODUCT_DEFINITION_SHAPE($,$,#424);
#12928=PRODUCT_DEFINITION_SHAPE($,$,#425);
#12929=PRODUCT_DEFINITION_SHAPE($,$,#426);
#12930=PRODUCT_DEFINITION_SHAPE($,$,#427);
#12931=PRODUCT_DEFINITION_SHAPE($,$,#428);
#12932=PRODUCT_DEFINITION_SHAPE($,$,#429);
#12933=PRODUCT_DEFINITION_SHAPE($,$,#430);
#12934=PRODUCT_DEFINITION_SHAPE($,$,#431);
#12935=PRODUCT_DEFINITION_SHAPE($,$,#432);
#12936=PRODUCT_DEFINITION_SHAPE($,$,#433);
#12937=PRODUCT_DEFINITION_SHAPE($,$,#434);
#12938=PRODUCT_DEFINITION_SHAPE($,$,#435);
#12939=PRODUCT_DEFINITION_SHAPE($,$,#436);
#12940=PRODUCT_DEFINITION_SHAPE($,$,#437);
#12941=PRODUCT_DEFINITION_SHAPE($,$,#438);
#12942=PRODUCT_DEFINITION_SHAPE($,$,#439);
#12943=PRODUCT_DEFINITION_SHAPE($,$,#440);
#12944=PRODUCT_DEFINITION_SHAPE($,$,#441);
#12945=PRODUCT_DEFINITION_SHAPE($,$,#442);
#12946=PRODUCT_DEFINITION_SHAPE($,$,#443);
#12947=PRODUCT_DEFINITION_SHAPE('',$,#13065);
#12948=PRODUCT_DEFINITION_SHAPE('',$,#13066);
#12949=PRODUCT_DEFINITION_SHAPE('',$,#13067);
#12950=PRODUCT_DEFINITION_SHAPE('',$,#13068);
#12951=PRODUCT_DEFINITION_SHAPE('',$,#13069);
#12952=PRODUCT_DEFINITION_SHAPE($,$,#444);
#12953=PRODUCT_DEFINITION_SHAPE($,$,#445);
#12954=PRODUCT_DEFINITION_SHAPE($,$,#446);
#12955=PRODUCT_DEFINITION_SHAPE($,$,#447);
#12956=PRODUCT_DEFINITION_SHAPE($,$,#448);
#12957=PRODUCT_DEFINITION_SHAPE($,$,#449);
#12958=PRODUCT_DEFINITION_SHAPE($,$,#450);
#12959=PRODUCT_DEFINITION_SHAPE($,$,#451);
#12960=PRODUCT_DEFINITION_SHAPE($,$,#452);
#12961=PRODUCT_DEFINITION_SHAPE($,$,#453);
#12962=PRODUCT_DEFINITION_SHAPE($,$,#454);
#12963=PRODUCT_DEFINITION_SHAPE($,$,#455);
#12964=PRODUCT_DEFINITION_SHAPE($,$,#456);
#12965=PRODUCT_DEFINITION_SHAPE($,$,#457);
#12966=PRODUCT_DEFINITION_SHAPE($,$,#458);
#12967=PRODUCT_DEFINITION_SHAPE($,$,#459);
#12968=PRODUCT_DEFINITION_SHAPE($,$,#460);
#12969=PRODUCT_DEFINITION_SHAPE($,$,#461);
#12970=PRODUCT_DEFINITION_SHAPE($,$,#462);
#12971=PRODUCT_DEFINITION_SHAPE($,$,#463);
#12972=PRODUCT_DEFINITION_SHAPE($,$,#464);
#12973=PRODUCT_DEFINITION_SHAPE($,$,#465);
#12974=PRODUCT_DEFINITION_SHAPE($,$,#466);
#12975=PRODUCT_DEFINITION_SHAPE($,$,#467);
#12976=PRODUCT_DEFINITION_SHAPE($,$,#468);
#12977=PRODUCT_DEFINITION_SHAPE($,$,#469);
#12978=PRODUCT_DEFINITION_SHAPE($,$,#470);
#12979=PRODUCT_DEFINITION_SHAPE($,$,#471);
#12980=PRODUCT_DEFINITION_SHAPE($,$,#472);
#12981=PRODUCT_DEFINITION_SHAPE($,$,#473);
#12982=PRODUCT_DEFINITION_SHAPE($,$,#474);
#12983=PRODUCT_DEFINITION_SHAPE($,$,#475);
#12984=PRODUCT_DEFINITION_SHAPE($,$,#476);
#12985=PRODUCT_DEFINITION_SHAPE($,$,#477);
#12986=PRODUCT_DEFINITION_SHAPE($,$,#478);
#12987=PRODUCT_DEFINITION_SHAPE($,$,#479);
#12988=PRODUCT_DEFINITION_SHAPE($,$,#480);
#12989=PRODUCT_DEFINITION_SHAPE($,$,#481);
#12990=PRODUCT_DEFINITION_SHAPE($,$,#482);
#12991=PRODUCT_DEFINITION_SHAPE($,$,#483);
#12992=PRODUCT_DEFINITION_SHAPE($,$,#484);
#12993=PRODUCT_DEFINITION_SHAPE($,$,#485);
#12994=PRODUCT_DEFINITION_SHAPE($,$,#486);
#12995=PRODUCT_DEFINITION_SHAPE($,$,#487);
#12996=PRODUCT_DEFINITION_SHAPE($,$,#488);
#12997=PRODUCT_DEFINITION_SHAPE($,$,#489);
#12998=PRODUCT_DEFINITION_SHAPE($,$,#490);
#12999=SHAPE_REPRESENTATION('',(#7741,#8485,#8486),#12769);
#13000=SHAPE_REPRESENTATION('',(#7742,#8274,#8275,#8276,#8277,#8278,#8279,
#8280,#8281,#8282,#8283,#8284,#8285,#8286,#8287,#8288,#8289,#8290,#8291,
#8292,#8293,#8294,#8295,#8296,#8297,#8298,#8299,#8300,#8301,#8302,#8303,
#8304,#8305,#8306,#8307,#8308,#8309,#8310,#8311,#8312,#8313,#8314,#8315,
#8316,#8317,#8318,#8319,#8320,#8321,#8322,#8323,#8324,#8325,#8326,#8327,
#8328,#8329,#8330,#8331,#8332,#8333,#8334,#8335,#8336,#8337,#8338,#8339,
#8340,#8341,#8342,#8343),#12770);
#13001=SHAPE_REPRESENTATION('',(#7743),#12771);
#13002=SHAPE_REPRESENTATION('',(#7768),#12772);
#13003=SHAPE_REPRESENTATION('',(#7793),#12773);
#13004=SHAPE_REPRESENTATION('',(#7806),#12774);
#13005=SHAPE_REPRESENTATION('',(#7819),#12775);
#13006=SHAPE_REPRESENTATION('',(#7826),#12776);
#13007=SHAPE_REPRESENTATION('',(#7833),#12777);
#13008=SHAPE_REPRESENTATION('',(#7846),#12778);
#13009=SHAPE_REPRESENTATION('',(#7859),#12779);
#13010=SHAPE_REPRESENTATION('',(#7866),#12780);
#13011=SHAPE_REPRESENTATION('',(#7873),#12781);
#13012=SHAPE_REPRESENTATION('',(#7902),#12782);
#13013=SHAPE_REPRESENTATION('',(#7909),#12783);
#13014=SHAPE_REPRESENTATION('',(#7938),#12784);
#13015=SHAPE_REPRESENTATION('',(#7945),#12785);
#13016=SHAPE_REPRESENTATION('',(#7995),#12786);
#13017=SHAPE_REPRESENTATION('',(#8038),#12787);
#13018=SHAPE_REPRESENTATION('',(#8064),#12788);
#13019=SHAPE_REPRESENTATION('',(#8085),#12789);
#13020=SHAPE_REPRESENTATION('',(#8109,#8440,#8441,#8442,#8443,#8444,#8445,
#8446,#8447,#8448,#8449,#8450,#8451,#8452,#8453,#8454,#8455,#8456,#8457,
#8458,#8459,#8460,#8461,#8462,#8463,#8464,#8465,#8466,#8467,#8468,#8469,
#8470,#8471,#8472,#8473,#8474,#8475,#8476,#8477,#8478,#8479,#8480,#8481,
#8482,#8483,#8484),#12790);
#13021=SHAPE_REPRESENTATION('',(#8110),#12791);
#13022=SHAPE_REPRESENTATION('',(#8174),#12792);
#13023=SHAPE_REPRESENTATION('',(#8183),#12793);
#13024=SHAPE_REPRESENTATION('',(#8198,#8260,#8261,#8262),#12794);
#13025=SHAPE_REPRESENTATION('',(#8199),#12795);
#13026=SHAPE_REPRESENTATION('',(#8238),#12796);
#13027=SHAPE_REPRESENTATION('',(#8249),#12797);
#13028=SHAPE_REPRESENTATION('',(#8263),#12798);
#13029=SHAPE_REPRESENTATION('',(#8344),#12799);
#13030=SHAPE_REPRESENTATION('',(#8370),#12800);
#13031=SHAPE_REPRESENTATION('',(#8379),#12801);
#13032=SHAPE_REPRESENTATION('',(#8405),#12802);
#13033=SHAPE_REPRESENTATION('',(#8416),#12803);
#13034=PRODUCT_DEFINITION_CONTEXT('part definition',#13141,'design');
#13035=PRODUCT_DEFINITION('PAT-033','PAT-033',#13070,
#13034);
#13036=PRODUCT_DEFINITION('Rail frame','Rail frame',#13071,#13034);
#13037=PRODUCT_DEFINITION('Rail adapter','Rail adapter',#13072,#13034);
#13038=PRODUCT_DEFINITION('Rail adapter (1)','Rail adapter (1)',#13073,#13034);
#13039=PRODUCT_DEFINITION('End tie plate','End tie plate',#13074,#13034);
#13040=PRODUCT_DEFINITION('Cross foot','Cross foot',#13075,#13034);
#13041=PRODUCT_DEFINITION('Bonded foot pad','Bonded foot pad',#13076,#13034);
#13042=PRODUCT_DEFINITION('Bonded foot pad (1)','Bonded foot pad (1)',#13077,
#13034);
#13043=PRODUCT_DEFINITION('End tie plate (1)','End tie plate (1)',#13078,
#13034);
#13044=PRODUCT_DEFINITION('Cross foot (1)','Cross foot (1)',#13079,#13034);
#13045=PRODUCT_DEFINITION('Bonded foot pad (2)','Bonded foot pad (2)',#13080,
#13034);
#13046=PRODUCT_DEFINITION('Bonded foot pad (3)','Bonded foot pad (3)',#13081,
#13034);
#13047=PRODUCT_DEFINITION('End stop beam','End stop beam',#13082,#13034);
#13048=PRODUCT_DEFINITION('Bonded stop pad','Bonded stop pad',#13083,#13034);
#13049=PRODUCT_DEFINITION('End stop beam (1)','End stop beam (1)',#13084,
#13034);
#13050=PRODUCT_DEFINITION('Bonded stop pad (1)','Bonded stop pad (1)',#13085,
#13034);
#13051=PRODUCT_DEFINITION('Slotted Extrusion - 20 x 20 x 400 mm',
'Slotted Extrusion - 20 x 20 x 400 mm',#13086,#13034);
#13052=PRODUCT_DEFINITION('Linear Guide Rail - 15 mm, 220 mm Long',
'Linear Guide Rail - 15 mm, 220 mm Long',#13087,#13034);
#13053=PRODUCT_DEFINITION('Cap Screw - M4x16','Cap Screw - M4x16',#13088,
#13034);
#13054=PRODUCT_DEFINITION('Captive slot nut','Captive slot nut',#13089,
#13034);
#13055=PRODUCT_DEFINITION('M5x14 Cap Screw','M5x14 Cap Screw',#13090,#13034);
#13056=PRODUCT_DEFINITION('Moving bridge','Moving bridge',#13091,#13034);
#13057=PRODUCT_DEFINITION('Bridge table','Bridge table',#13092,#13034);
#13058=PRODUCT_DEFINITION('Manual grip','Manual grip',#13093,#13034);
#13059=PRODUCT_DEFINITION('Cable bracket','Cable bracket',#13094,#13034);
#13060=PRODUCT_DEFINITION('Flanged Linear Guide Carriage - 15 mm',
'Flanged Linear Guide Carriage - 15 mm',#13095,#13034);
#13061=PRODUCT_DEFINITION('Block','Block',#13096,#13034);
#13062=PRODUCT_DEFINITION('End cap +','End cap +',#13097,#13034);
#13063=PRODUCT_DEFINITION('End cap','End cap',#13098,#13034);
#13064=PRODUCT_DEFINITION('Flat Washer - M5','Flat Washer - M5',#13099,
#13034);
#13065=PRODUCT_DEFINITION('Cap Screw - M5x20','Cap Screw - M5x20',#13100,
#13034);
#13066=PRODUCT_DEFINITION('Flat Washer - M6','Flat Washer - M6',#13101,
#13034);
#13067=PRODUCT_DEFINITION('Cap Screw - M6x25','Cap Screw - M6x25',#13102,
#13034);
#13068=PRODUCT_DEFINITION('Flat Washer - M4','Flat Washer - M4',#13103,
#13034);
#13069=PRODUCT_DEFINITION('M4x10 Cap Screw','M4x10 Cap Screw',#13104,#13034);
#13070=PRODUCT_DEFINITION_FORMATION('',$,#13143);
#13071=PRODUCT_DEFINITION_FORMATION('',$,#13144);
#13072=PRODUCT_DEFINITION_FORMATION('',$,#13145);
#13073=PRODUCT_DEFINITION_FORMATION('',$,#13146);
#13074=PRODUCT_DEFINITION_FORMATION('',$,#13147);
#13075=PRODUCT_DEFINITION_FORMATION('',$,#13148);
#13076=PRODUCT_DEFINITION_FORMATION('',$,#13149);
#13077=PRODUCT_DEFINITION_FORMATION('',$,#13150);
#13078=PRODUCT_DEFINITION_FORMATION('',$,#13151);
#13079=PRODUCT_DEFINITION_FORMATION('',$,#13152);
#13080=PRODUCT_DEFINITION_FORMATION('',$,#13153);
#13081=PRODUCT_DEFINITION_FORMATION('',$,#13154);
#13082=PRODUCT_DEFINITION_FORMATION('',$,#13155);
#13083=PRODUCT_DEFINITION_FORMATION('',$,#13156);
#13084=PRODUCT_DEFINITION_FORMATION('',$,#13157);
#13085=PRODUCT_DEFINITION_FORMATION('',$,#13158);
#13086=PRODUCT_DEFINITION_FORMATION('',$,#13159);
#13087=PRODUCT_DEFINITION_FORMATION('',$,#13160);
#13088=PRODUCT_DEFINITION_FORMATION('',$,#13161);
#13089=PRODUCT_DEFINITION_FORMATION('',$,#13162);
#13090=PRODUCT_DEFINITION_FORMATION('',$,#13163);
#13091=PRODUCT_DEFINITION_FORMATION('',$,#13164);
#13092=PRODUCT_DEFINITION_FORMATION('',$,#13165);
#13093=PRODUCT_DEFINITION_FORMATION('',$,#13166);
#13094=PRODUCT_DEFINITION_FORMATION('',$,#13167);
#13095=PRODUCT_DEFINITION_FORMATION('',$,#13168);
#13096=PRODUCT_DEFINITION_FORMATION('',$,#13169);
#13097=PRODUCT_DEFINITION_FORMATION('',$,#13170);
#13098=PRODUCT_DEFINITION_FORMATION('',$,#13171);
#13099=PRODUCT_DEFINITION_FORMATION('',$,#13172);
#13100=PRODUCT_DEFINITION_FORMATION('',$,#13173);
#13101=PRODUCT_DEFINITION_FORMATION('',$,#13174);
#13102=PRODUCT_DEFINITION_FORMATION('',$,#13175);
#13103=PRODUCT_DEFINITION_FORMATION('',$,#13176);
#13104=PRODUCT_DEFINITION_FORMATION('',$,#13177);
#13105=PRODUCT_RELATED_PRODUCT_CATEGORY('PAT-033','PAT-033',(#13143));
#13106=PRODUCT_RELATED_PRODUCT_CATEGORY('Rail frame','Rail frame',(#13144));
#13107=PRODUCT_RELATED_PRODUCT_CATEGORY('Rail adapter','Rail adapter',(#13145));
#13108=PRODUCT_RELATED_PRODUCT_CATEGORY('Rail adapter (1)',
'Rail adapter (1)',(#13146));
#13109=PRODUCT_RELATED_PRODUCT_CATEGORY('End tie plate','End tie plate',
(#13147));
#13110=PRODUCT_RELATED_PRODUCT_CATEGORY('Cross foot','Cross foot',(#13148));
#13111=PRODUCT_RELATED_PRODUCT_CATEGORY('Bonded foot pad',
'Bonded foot pad',(#13149));
#13112=PRODUCT_RELATED_PRODUCT_CATEGORY('Bonded foot pad (1)',
'Bonded foot pad (1)',(#13150));
#13113=PRODUCT_RELATED_PRODUCT_CATEGORY('End tie plate (1)',
'End tie plate (1)',(#13151));
#13114=PRODUCT_RELATED_PRODUCT_CATEGORY('Cross foot (1)',
'Cross foot (1)',(#13152));
#13115=PRODUCT_RELATED_PRODUCT_CATEGORY('Bonded foot pad (2)',
'Bonded foot pad (2)',(#13153));
#13116=PRODUCT_RELATED_PRODUCT_CATEGORY('Bonded foot pad (3)',
'Bonded foot pad (3)',(#13154));
#13117=PRODUCT_RELATED_PRODUCT_CATEGORY('End stop beam','End stop beam',
(#13155));
#13118=PRODUCT_RELATED_PRODUCT_CATEGORY('Bonded stop pad',
'Bonded stop pad',(#13156));
#13119=PRODUCT_RELATED_PRODUCT_CATEGORY('End stop beam (1)',
'End stop beam (1)',(#13157));
#13120=PRODUCT_RELATED_PRODUCT_CATEGORY('Bonded stop pad (1)',
'Bonded stop pad (1)',(#13158));
#13121=PRODUCT_RELATED_PRODUCT_CATEGORY(
'Slotted Extrusion - 20 x 20 x 400 mm',
'Slotted Extrusion - 20 x 20 x 400 mm',(#13159));
#13122=PRODUCT_RELATED_PRODUCT_CATEGORY(
'Linear Guide Rail - 15 mm, 220 mm Long',
'Linear Guide Rail - 15 mm, 220 mm Long',(#13160));
#13123=PRODUCT_RELATED_PRODUCT_CATEGORY('Cap Screw - M4x16',
'Cap Screw - M4x16',(#13161));
#13124=PRODUCT_RELATED_PRODUCT_CATEGORY('Captive slot nut',
'Captive slot nut',(#13162));
#13125=PRODUCT_RELATED_PRODUCT_CATEGORY('M5x14 Cap Screw',
'M5x14 Cap Screw',(#13163));
#13126=PRODUCT_RELATED_PRODUCT_CATEGORY('Moving bridge','Moving bridge',
(#13164));
#13127=PRODUCT_RELATED_PRODUCT_CATEGORY('Bridge table','Bridge table',(#13165));
#13128=PRODUCT_RELATED_PRODUCT_CATEGORY('Manual grip','Manual grip',(#13166));
#13129=PRODUCT_RELATED_PRODUCT_CATEGORY('Cable bracket','Cable bracket',
(#13167));
#13130=PRODUCT_RELATED_PRODUCT_CATEGORY(
'Flanged Linear Guide Carriage - 15 mm',
'Flanged Linear Guide Carriage - 15 mm',(#13168));
#13131=PRODUCT_RELATED_PRODUCT_CATEGORY('Block','Block',(#13169));
#13132=PRODUCT_RELATED_PRODUCT_CATEGORY('End cap +','End cap +',(#13170));
#13133=PRODUCT_RELATED_PRODUCT_CATEGORY('End cap','End cap',(#13171));
#13134=PRODUCT_RELATED_PRODUCT_CATEGORY('Flat Washer - M5',
'Flat Washer - M5',(#13172));
#13135=PRODUCT_RELATED_PRODUCT_CATEGORY('Cap Screw - M5x20',
'Cap Screw - M5x20',(#13173));
#13136=PRODUCT_RELATED_PRODUCT_CATEGORY('Flat Washer - M6',
'Flat Washer - M6',(#13174));
#13137=PRODUCT_RELATED_PRODUCT_CATEGORY('Cap Screw - M6x25',
'Cap Screw - M6x25',(#13175));
#13138=PRODUCT_RELATED_PRODUCT_CATEGORY('Flat Washer - M4',
'Flat Washer - M4',(#13176));
#13139=PRODUCT_RELATED_PRODUCT_CATEGORY('M4x10 Cap Screw',
'M4x10 Cap Screw',(#13177));
#13140=APPLICATION_PROTOCOL_DEFINITION('international standard',
'automotive_design',2009,#13141);
#13141=APPLICATION_CONTEXT(
'Core Data for Automotive Mechanical Design Process');
#13142=PRODUCT_CONTEXT('part definition',#13141,'mechanical');
#13143=PRODUCT('PAT-033','PAT-033',
'PAT-033',(#13142));
#13144=PRODUCT('Rail frame','Rail frame','Rail frame',(#13142));
#13145=PRODUCT('Rail adapter','Rail adapter','Rail adapter',(#13142));
#13146=PRODUCT('Rail adapter (1)','Rail adapter (1)','Rail adapter (1)',(#13142));
#13147=PRODUCT('End tie plate','End tie plate','End tie plate',(#13142));
#13148=PRODUCT('Cross foot','Cross foot','Cross foot',(#13142));
#13149=PRODUCT('Bonded foot pad','Bonded foot pad','Bonded foot pad',(#13142));
#13150=PRODUCT('Bonded foot pad (1)','Bonded foot pad (1)',
'Bonded foot pad (1)',(#13142));
#13151=PRODUCT('End tie plate (1)','End tie plate (1)','End tie plate (1)',(#13142));
#13152=PRODUCT('Cross foot (1)','Cross foot (1)','Cross foot (1)',(#13142));
#13153=PRODUCT('Bonded foot pad (2)','Bonded foot pad (2)',
'Bonded foot pad (2)',(#13142));
#13154=PRODUCT('Bonded foot pad (3)','Bonded foot pad (3)',
'Bonded foot pad (3)',(#13142));
#13155=PRODUCT('End stop beam','End stop beam','End stop beam',(#13142));
#13156=PRODUCT('Bonded stop pad','Bonded stop pad','Bonded stop pad',(#13142));
#13157=PRODUCT('End stop beam (1)','End stop beam (1)','End stop beam (1)',(#13142));
#13158=PRODUCT('Bonded stop pad (1)','Bonded stop pad (1)',
'Bonded stop pad (1)',(#13142));
#13159=PRODUCT('Slotted Extrusion - 20 x 20 x 400 mm',
'Slotted Extrusion - 20 x 20 x 400 mm',
'Slotted Extrusion - 20 x 20 x 400 mm',(#13142));
#13160=PRODUCT('Linear Guide Rail - 15 mm, 220 mm Long',
'Linear Guide Rail - 15 mm, 220 mm Long',
'Linear Guide Rail - 15 mm, 220 mm Long',(#13142));
#13161=PRODUCT('Cap Screw - M4x16','Cap Screw - M4x16',
'Cap Screw - M4x16',(#13142));
#13162=PRODUCT('Captive slot nut','Captive slot nut','Captive slot nut',
(#13142));
#13163=PRODUCT('M5x14 Cap Screw','M5x14 Cap Screw','M5x14 Cap Screw',(#13142));
#13164=PRODUCT('Moving bridge','Moving bridge','Moving bridge',(#13142));
#13165=PRODUCT('Bridge table','Bridge table','Bridge table',(#13142));
#13166=PRODUCT('Manual grip','Manual grip','Manual grip',(#13142));
#13167=PRODUCT('Cable bracket','Cable bracket','Cable bracket',(#13142));
#13168=PRODUCT('Flanged Linear Guide Carriage - 15 mm',
'Flanged Linear Guide Carriage - 15 mm',
'Flanged Linear Guide Carriage - 15 mm',(#13142));
#13169=PRODUCT('Block','Block','Block',(#13142));
#13170=PRODUCT('End cap +','End cap +','End cap +',(#13142));
#13171=PRODUCT('End cap','End cap','End cap',(#13142));
#13172=PRODUCT('Flat Washer - M5','Flat Washer - M5','Flat Washer - M5',
(#13142));
#13173=PRODUCT('Cap Screw - M5x20','Cap Screw - M5x20',
'Cap Screw - M5x20',(#13142));
#13174=PRODUCT('Flat Washer - M6','Flat Washer - M6','Flat Washer - M6',
(#13142));
#13175=PRODUCT('Cap Screw - M6x25','Cap Screw - M6x25',
'Cap Screw - M6x25',(#13142));
#13176=PRODUCT('Flat Washer - M4','Flat Washer - M4','Flat Washer - M4',
(#13142));
#13177=PRODUCT('M4x10 Cap Screw','M4x10 Cap Screw','M4x10 Cap Screw',(#13142));
#13178=PRESENTATION_STYLE_ASSIGNMENT((#13184));
#13179=PRESENTATION_STYLE_ASSIGNMENT((#13185));
#13180=PRESENTATION_STYLE_ASSIGNMENT((#13186));
#13181=PRESENTATION_STYLE_ASSIGNMENT((#13187));
#13182=PRESENTATION_STYLE_ASSIGNMENT((#13188));
#13183=PRESENTATION_STYLE_ASSIGNMENT((#13189));
#13184=SURFACE_STYLE_USAGE(.BOTH.,#13190);
#13185=SURFACE_STYLE_USAGE(.BOTH.,#13191);
#13186=SURFACE_STYLE_USAGE(.BOTH.,#13192);
#13187=SURFACE_STYLE_USAGE(.BOTH.,#13193);
#13188=SURFACE_STYLE_USAGE(.BOTH.,#13194);
#13189=SURFACE_STYLE_USAGE(.BOTH.,#13195);
#13190=SURFACE_SIDE_STYLE('',(#13196));
#13191=SURFACE_SIDE_STYLE('',(#13197));
#13192=SURFACE_SIDE_STYLE('',(#13198));
#13193=SURFACE_SIDE_STYLE('',(#13199));
#13194=SURFACE_SIDE_STYLE('',(#13200));
#13195=SURFACE_SIDE_STYLE('',(#13201));
#13196=SURFACE_STYLE_FILL_AREA(#13202);
#13197=SURFACE_STYLE_FILL_AREA(#13203);
#13198=SURFACE_STYLE_FILL_AREA(#13204);
#13199=SURFACE_STYLE_FILL_AREA(#13205);
#13200=SURFACE_STYLE_FILL_AREA(#13206);
#13201=SURFACE_STYLE_FILL_AREA(#13207);
#13202=FILL_AREA_STYLE('Steel - Satin',(#13208));
#13203=FILL_AREA_STYLE('CAD Library Painted - Steel gray',(#13209));
#13204=FILL_AREA_STYLE('CAD Library Painted - Engineering blue',(#13210));
#13205=FILL_AREA_STYLE('CAD Library Painted - Deep blue',(#13211));
#13206=FILL_AREA_STYLE('CAD Library Painted - Graphite',(#13212));
#13207=FILL_AREA_STYLE('CAD Library Painted - Light blue',(#13213));
#13208=FILL_AREA_STYLE_COLOUR('Steel - Satin',#13214);
#13209=FILL_AREA_STYLE_COLOUR('CAD Library Painted - Steel gray',#13215);
#13210=FILL_AREA_STYLE_COLOUR('CAD Library Painted - Engineering blue',
#13216);
#13211=FILL_AREA_STYLE_COLOUR('CAD Library Painted - Deep blue',#13217);
#13212=FILL_AREA_STYLE_COLOUR('CAD Library Painted - Graphite',#13218);
#13213=FILL_AREA_STYLE_COLOUR('CAD Library Painted - Light blue',#13219);
#13214=COLOUR_RGB('Steel - Satin',0.627450980392157,0.627450980392157,0.627450980392157);
#13215=COLOUR_RGB('CAD Library Painted - Steel gray',0.592156862745098,
0.631372549019608,0.67843137254902);
#13216=COLOUR_RGB('CAD Library Painted - Engineering blue',0.12156862745098,
0.356862745098039,0.6);
#13217=COLOUR_RGB('CAD Library Painted - Deep blue',0.0784313725490196,
0.203921568627451,0.349019607843137);
#13218=COLOUR_RGB('CAD Library Painted - Graphite',0.168627450980392,0.192156862745098,
0.231372549019608);
#13219=COLOUR_RGB('CAD Library Painted - Light blue',0.286274509803922,
0.552941176470588,0.780392156862745);
#13220=COLOUR_RGB('Dark Blue',0.08,0.2,0.34);
#13221=FILL_AREA_STYLE_COLOUR('',#13220);
#13222=FILL_AREA_STYLE('',(#13221));
#13223=SURFACE_STYLE_FILL_AREA(#13222);
#13224=SURFACE_SIDE_STYLE('',(#13223));
#13225=SURFACE_STYLE_USAGE(.BOTH.,#13224);
#13226=PRESENTATION_STYLE_ASSIGNMENT((#13225));
#13227=COLOUR_RGB('Light Blue',0.38,0.62,0.78);
#13228=FILL_AREA_STYLE_COLOUR('',#13227);
#13229=FILL_AREA_STYLE('',(#13228));
#13230=SURFACE_STYLE_FILL_AREA(#13229);
#13231=SURFACE_SIDE_STYLE('',(#13230));
#13232=SURFACE_STYLE_USAGE(.BOTH.,#13231);
#13233=PRESENTATION_STYLE_ASSIGNMENT((#13232));
#13234=COLOUR_RGB('Sky Blue',0.24,0.69,0.87);
#13235=FILL_AREA_STYLE_COLOUR('',#13234);
#13236=FILL_AREA_STYLE('',(#13235));
#13237=SURFACE_STYLE_FILL_AREA(#13236);
#13238=SURFACE_SIDE_STYLE('',(#13237));
#13239=SURFACE_STYLE_USAGE(.BOTH.,#13238);
#13240=PRESENTATION_STYLE_ASSIGNMENT((#13239));
#13241=COLOUR_RGB('Grey',0.48,0.52,0.57);
#13242=FILL_AREA_STYLE_COLOUR('',#13241);
#13243=FILL_AREA_STYLE('',(#13242));
#13244=SURFACE_STYLE_FILL_AREA(#13243);
#13245=SURFACE_SIDE_STYLE('',(#13244));
#13246=SURFACE_STYLE_USAGE(.BOTH.,#13245);
#13247=PRESENTATION_STYLE_ASSIGNMENT((#13246));
#13248=COLOUR_RGB('Black',0.12,0.14,0.17);
#13249=FILL_AREA_STYLE_COLOUR('',#13248);
#13250=FILL_AREA_STYLE('',(#13249));
#13251=SURFACE_STYLE_FILL_AREA(#13250);
#13252=SURFACE_SIDE_STYLE('',(#13251));
#13253=SURFACE_STYLE_USAGE(.BOTH.,#13252);
#13254=PRESENTATION_STYLE_ASSIGNMENT((#13253));
#13255=COLOUR_RGB('Off White',0.89,0.88,0.83);
#13256=FILL_AREA_STYLE_COLOUR('',#13255);
#13257=FILL_AREA_STYLE('',(#13256));
#13258=SURFACE_STYLE_FILL_AREA(#13257);
#13259=SURFACE_SIDE_STYLE('',(#13258));
#13260=SURFACE_STYLE_USAGE(.BOTH.,#13259);
#13261=PRESENTATION_STYLE_ASSIGNMENT((#13260));
ENDSEC;
END-ISO-10303-21;
